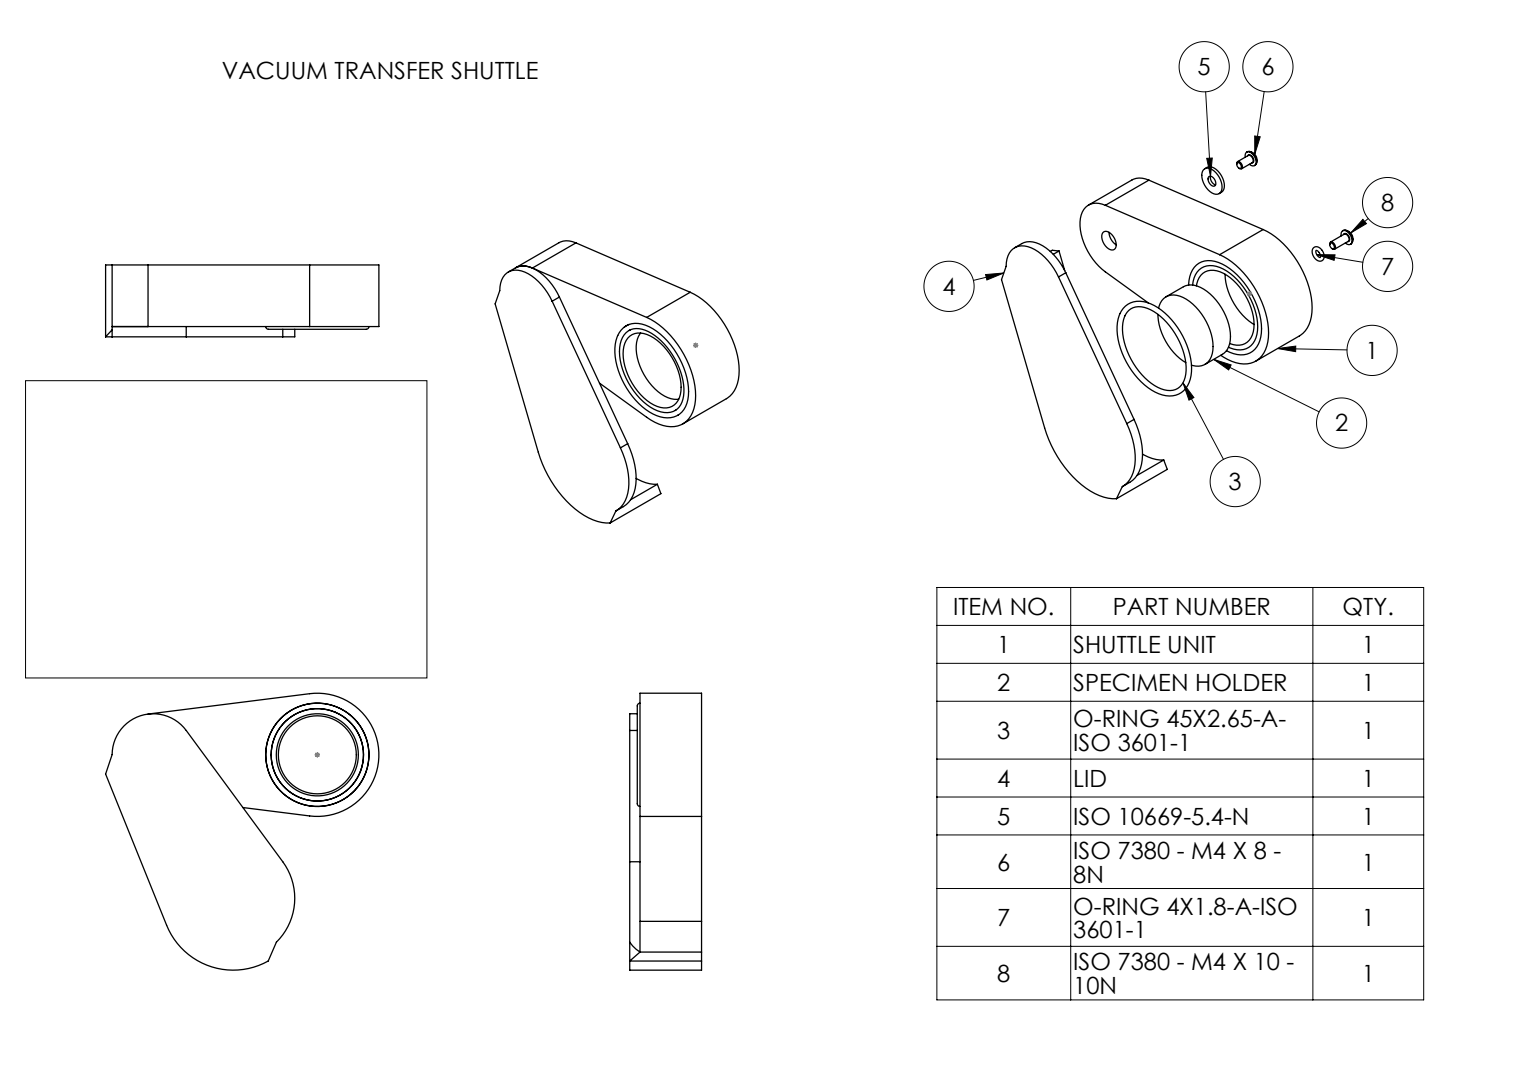
ISO-10303-21;
HEADER;
FILE_DESCRIPTION (('STEP AP214'),
    '1' );
FILE_NAME ('MAS-190',
    '2026-10-24T08:20:21',
    ( '' ),
    ( '' ),
    'SwSTEP 2.0',
    'SolidWorks 2026',
    '' );
FILE_SCHEMA (( 'AUTOMOTIVE_DESIGN' ));
ENDSEC;

DATA;
#1 = VERTEX_POINT ( 'NONE', #624 ) ;
#2 = DIRECTION ( 'NONE',  ( -1.000000000000000000, 0.000000000000000000, 0.000000000000000000 ) ) ;
#3 = CARTESIAN_POINT ( 'NONE',  ( 1.300000000000000044, 1.443375672974065216, 7.222237291452134449E-31 ) ) ;
#4 = DIRECTION ( 'NONE',  ( -0.000000000000000000, -0.000000000000000000, -1.000000000000000000 ) ) ;
#5 = ORIENTED_EDGE ( 'NONE', *, *, #1076, .T. ) ;
#6 = CARTESIAN_POINT ( 'NONE',  ( 0.000000000000000000, 0.000000000000000000, -15.70000000000000284 ) ) ;
#7 = PLANE ( 'NONE',  #3620 ) ;
#8 = DIRECTION ( 'NONE',  ( 1.000000000000000000, 0.000000000000000000, 0.000000000000000000 ) ) ;
#9 = DIRECTION ( 'NONE',  ( 0.000000000000000000, 0.000000000000000000, 1.000000000000000000 ) ) ;
#10 = ORIENTED_EDGE ( 'NONE', *, *, #2629, .T. ) ;
#11 = ORIENTED_EDGE ( 'NONE', *, *, #3486, .F. ) ;
#12 = LINE ( 'NONE', #3823, #2390 ) ;
#13 = ORIENTED_EDGE ( 'NONE', *, *, #231, .T. ) ;
#14 = CARTESIAN_POINT ( 'NONE',  ( 1.820000000000000062, 0.000000000000000000, 0.000000000000000000 ) ) ;
#15 = VERTEX_POINT ( 'NONE', #148 ) ;
#16 = CARTESIAN_POINT ( 'NONE',  ( 0.000000000000000000, 8.572527594031473190E-16, -7.000000000000000000 ) ) ;
#17 = DIRECTION ( 'NONE',  ( -1.000000000000000000, -1.224646799147353454E-16, 0.000000000000000000 ) ) ;
#18 = VECTOR ( 'NONE', #3561, 1000.000000000000114 ) ;
#19 = DIRECTION ( 'NONE',  ( -0.7071067811865492381, 8.659560562354911904E-17, -0.7071067811865457964 ) ) ;
#20 = AXIS2_PLACEMENT_3D ( 'NONE', #499, #4, #521 ) ;
#21 = EDGE_LOOP ( 'NONE', ( #2313, #294, #1297, #1026, #1998 ) ) ;
#22 = CARTESIAN_POINT ( 'NONE',  ( 0.000000000000000000, 0.000000000000000000, -30.00000000000000000 ) ) ;
#23 = LINE ( 'NONE', #2105, #2068 ) ;
#24 = VECTOR ( 'NONE', #1964, 1000.000000000000000 ) ;
#25 = VECTOR ( 'NONE', #749, 1000.000000000000114 ) ;
#26 = EDGE_CURVE ( 'NONE', #192, #3050, #3399, .T. ) ;
#27 = CARTESIAN_POINT ( 'NONE',  ( -85.00000000000000000, 6.123233995736770227E-16, 0.000000000000000000 ) ) ;
#28 = EDGE_LOOP ( 'NONE', ( #1681, #1312, #3374, #1579 ) ) ;
#29 = VECTOR ( 'NONE', #2095, 1000.000000000000000 ) ;
#30 = ORIENTED_EDGE ( 'NONE', *, *, #1022, .T. ) ;
#31 = EDGE_LOOP ( 'NONE', ( #3797, #723, #569, #2340, #3263 ) ) ;
#32 = LINE ( 'NONE', #599, #2631 ) ;
#33 = CIRCLE ( 'NONE', #906, 20.00000000000000355 ) ;
#34 = EDGE_CURVE ( 'NONE', #3645, #1107, #2841, .T. ) ;
#35 = CIRCLE ( 'NONE', #2208, 22.50000000000000355 ) ;
#36 = ORIENTED_EDGE ( 'NONE', *, *, #1121, .F. ) ;
#37 = FACE_OUTER_BOUND ( 'NONE', #2030, .T. ) ;
#38 = CARTESIAN_POINT ( 'NONE',  ( 0.000000000000000000, -0.7216878364870318308, -1.250000000000000000 ) ) ;
#39 = CARTESIAN_POINT ( 'NONE',  ( 0.000000000000000000, 0.000000000000000000, -24.90000000000000568 ) ) ;
#40 = COLOUR_RGB ( '',0.8941176470588234615, 0.8941176470588234615, 0.8941176470588234615 ) ;
#41 = PRODUCT_DEFINITION_SHAPE ( 'NONE', 'NONE',  #583 ) ;
#42 = DIRECTION ( 'NONE',  ( 0.000000000000000000, 0.000000000000000000, 1.000000000000000000 ) ) ;
#43 = PLANE ( 'NONE',  #1656 ) ;
#44 = DIRECTION ( 'NONE',  ( -0.000000000000000000, 0.5000000000000002220, -0.8660254037844384856 ) ) ;
#45 =( LENGTH_UNIT ( ) NAMED_UNIT ( * ) SI_UNIT ( .MILLI., .METRE. ) );
#46 = EDGE_CURVE ( 'NONE', #2758, #1577, #1662, .T. ) ;
#47 = PLANE ( 'NONE',  #2813 ) ;
#48 = CARTESIAN_POINT ( 'NONE',  ( 1.300000000000000044, 0.000000000000000000, 0.000000000000000000 ) ) ;
#49 = EDGE_CURVE ( 'NONE', #3210, #3147, #1369, .T. ) ;
#50 = ORIENTED_EDGE ( 'NONE', *, *, #3736, .T. ) ;
#51 = FACE_OUTER_BOUND ( 'NONE', #2108, .T. ) ;
#52 = VERTEX_POINT ( 'NONE', #3188 ) ;
#53 = CARTESIAN_POINT ( 'NONE',  ( 2.021687836487040535, 0.000000000000000000, 2.168404344971008868E-16 ) ) ;
#54 = ORIENTED_EDGE ( 'NONE', *, *, #3614, .T. ) ;
#55 = DIRECTION ( 'NONE',  ( 1.000000000000000000, 0.000000000000000000, 0.000000000000000000 ) ) ;
#56 = DIRECTION ( 'NONE',  ( -1.000000000000000000, 0.000000000000000000, -0.000000000000000000 ) ) ;
#57 = CARTESIAN_POINT ( 'NONE',  ( 2.200000000000000178, 0.000000000000000000, 3.799999999999999378 ) ) ;
#58 = DIRECTION ( 'NONE',  ( 0.1250000000000000833, 0.9921567416492215186, -0.000000000000000000 ) ) ;
#59 = DIRECTION ( 'NONE',  ( 1.000000000000000000, 0.000000000000000000, 0.000000000000000000 ) ) ;
#60 = DIRECTION ( 'NONE',  ( 1.000000000000000000, 0.000000000000000000, -0.000000000000000000 ) ) ;
#61 = DIRECTION ( 'NONE',  ( -1.000000000000000000, -1.224646799147352961E-16, 0.000000000000000000 ) ) ;
#62 = AXIS2_PLACEMENT_3D ( 'NONE', #1095, #2604, #3467 ) ;
#63 = ORIENTED_EDGE ( 'NONE', *, *, #1690, .T. ) ;
#64 = DIRECTION ( 'NONE',  ( -1.000000000000000000, 0.000000000000000000, 0.000000000000000000 ) ) ;
#65 = EDGE_LOOP ( 'NONE', ( #2892, #2887, #2094, #2492 ) ) ;
#66 = CARTESIAN_POINT ( 'NONE',  ( -80.00000000000000000, 0.000000000000000000, -5.000000000000000000 ) ) ;
#67 = ORIENTED_EDGE ( 'NONE', *, *, #1212, .F. ) ;
#68 = CARTESIAN_POINT ( 'NONE',  ( -80.00000000000000000, 0.000000000000000000, 0.000000000000000000 ) ) ;
#69 = FACE_OUTER_BOUND ( 'NONE', #2614, .T. ) ;
#70 = DIRECTION ( 'NONE',  ( -1.000000000000000000, 0.000000000000000000, 0.000000000000000000 ) ) ;
#71 = AXIS2_PLACEMENT_3D ( 'NONE', #2197, #416, #1075 ) ;
#72 = CARTESIAN_POINT ( 'NONE',  ( 1.300000000000000044, -0.7216878364870317197, -1.250000000000000000 ) ) ;
#73 = CARTESIAN_POINT ( 'NONE',  ( -80.00000000000000000, 0.000000000000000000, -5.000000000000000000 ) ) ;
#74 = TOROIDAL_SURFACE ( 'NONE', #3494, 23.82500000000000284, 1.324999999999999956 ) ;
#75 = VECTOR ( 'NONE', #2409, 1000.000000000000114 ) ;
#76 = FACE_OUTER_BOUND ( 'NONE', #2053, .T. ) ;
#77 = DIRECTION ( 'NONE',  ( -1.000000000000000000, 0.000000000000000000, 0.000000000000000000 ) ) ;
#78 = EDGE_CURVE ( 'NONE', #2558, #3229, #1744, .T. ) ;
#79 = VECTOR ( 'NONE', #1201, 1000.000000000000000 ) ;
#80 = VERTEX_POINT ( 'NONE', #800 ) ;
#81 = SURFACE_STYLE_USAGE ( .BOTH. , #2750 ) ;
#82 = ORIENTED_EDGE ( 'NONE', *, *, #2472, .F. ) ;
#83 = AXIS2_PLACEMENT_3D ( 'NONE', #3751, #2911, #1411 ) ;
#84 = DIRECTION ( 'NONE',  ( -1.000000000000000000, -0.000000000000000000, -0.000000000000000000 ) ) ;
#85 = CARTESIAN_POINT ( 'NONE',  ( 0.000000000000000000, 0.000000000000000000, -30.00000000000000000 ) ) ;
#86 = ORIENTED_EDGE ( 'NONE', *, *, #1066, .F. ) ;
#87 = CARTESIAN_POINT ( 'NONE',  ( 0.000000000000000000, 0.000000000000000000, 0.000000000000000000 ) ) ;
#88 = VECTOR ( 'NONE', #755, 999.9999999999998863 ) ;
#89 = CARTESIAN_POINT ( 'NONE',  ( 0.000000000000000000, 0.000000000000000000, -15.70000000000000284 ) ) ;
#90 = AXIS2_PLACEMENT_3D ( 'NONE', #3655, #2505, #3718 ) ;
#91 = LINE ( 'NONE', #72, #1895 ) ;
#92 = CARTESIAN_POINT ( 'NONE',  ( 28.92857142857272379, 7.945926950454914817, 5.000000000000000000 ) ) ;
#93 = AXIS2_PLACEMENT_3D ( 'NONE', #3300, #56, #338 ) ;
#94 = CARTESIAN_POINT ( 'NONE',  ( 0.000000000000000000, 0.000000000000000000, 1.999999999999999112 ) ) ;
#95 = CARTESIAN_POINT ( 'NONE',  ( 1.600000000000000089, 0.000000000000000000, 0.000000000000000000 ) ) ;
#96 = ORIENTED_EDGE ( 'NONE', *, *, #3202, .F. ) ;
#97 = ORIENTED_EDGE ( 'NONE', *, *, #3095, .F. ) ;
#98 = CARTESIAN_POINT ( 'NONE',  ( 1.300000000000000044, -0.7216878364870317197, -1.250000000000000000 ) ) ;
#99 = ADVANCED_FACE ( 'NONE', ( #3496 ), #810, .T. ) ;
#100 = EDGE_CURVE ( 'NONE', #2912, #2597, #2303, .T. ) ;
#101 = CARTESIAN_POINT ( 'NONE',  ( -85.00000000000000000, 0.000000000000000000, 0.001000000000000132727 ) ) ;
#102 = VERTEX_POINT ( 'NONE', #209 ) ;
#103 = CARTESIAN_POINT ( 'NONE',  ( -90.00000000000000000, 0.000000000000000000, -4.999999999999997335 ) ) ;
#104 = FACE_OUTER_BOUND ( 'NONE', #1200, .T. ) ;
#105 = DIRECTION ( 'NONE',  ( -1.000000000000000000, 0.000000000000000000, 0.000000000000000000 ) ) ;
#106 = EDGE_CURVE ( 'NONE', #1824, #3785, #3518, .T. ) ;
#107 = CARTESIAN_POINT ( 'NONE',  ( -82.50000000000000000, -19.84313483298442904, 0.000000000000000000 ) ) ;
#108 = ORIENTED_EDGE ( 'NONE', *, *, #561, .F. ) ;
#109 = DIRECTION ( 'NONE',  ( -1.000000000000000000, -0.000000000000000000, -0.000000000000000000 ) ) ;
#110 = ADVANCED_FACE ( 'NONE', ( #3446, #2287 ), #2899, .F. ) ;
#111 = DIRECTION ( 'NONE',  ( -0.000000000000000000, -0.000000000000000000, -1.000000000000000000 ) ) ;
#112 = PLANE ( 'NONE',  #3812 ) ;
#113 = ORIENTED_EDGE ( 'NONE', *, *, #1158, .T. ) ;
#114 =( NAMED_UNIT ( * ) SI_UNIT ( $, .STERADIAN. ) SOLID_ANGLE_UNIT ( ) );
#115 = ORIENTED_EDGE ( 'NONE', *, *, #3737, .T. ) ;
#116 = PLANE ( 'NONE',  #1634 ) ;
#117 = CARTESIAN_POINT ( 'NONE',  ( 1.820000000000000062, 3.799999999999999378, 0.000000000000000000 ) ) ;
#118 = ORIENTED_EDGE ( 'NONE', *, *, #270, .T. ) ;
#119 = DIRECTION ( 'NONE',  ( -0.000000000000000000, 0.000000000000000000, 1.000000000000000000 ) ) ;
#120 = CARTESIAN_POINT ( 'NONE',  ( 12.20000000000000107, 0.000000000000000000, 0.000000000000000000 ) ) ;
#121 = PLANE ( 'NONE',  #644 ) ;
#122 = CARTESIAN_POINT ( 'NONE',  ( 9.809999999999998721, 0.000000000000000000, 0.000000000000000000 ) ) ;
#123 = EDGE_LOOP ( 'NONE', ( #2898, #2234 ) ) ;
#124 = LINE ( 'NONE', #2843, #702 ) ;
#125 = SURFACE_STYLE_USAGE ( .BOTH. , #2878 ) ;
#126 = CIRCLE ( 'NONE', #71, 1.999999999999999556 ) ;
#127 = APPLICATION_PROTOCOL_DEFINITION ( 'draft international standard', 'automotive_design', 1998, #1375 ) ;
#128 = CARTESIAN_POINT ( 'NONE',  ( -80.00000000000000000, 0.000000000000000000, -30.00000000000000000 ) ) ;
#129 = CARTESIAN_POINT ( 'NONE',  ( 1.300000000000000044, 0.7216878364870328300, -1.250000000000000000 ) ) ;
#130 = COLOUR_RGB ( '',0.8941176470588234615, 0.8941176470588234615, 0.8941176470588234615 ) ;
#131 = VECTOR ( 'NONE', #1399, 1000.000000000000000 ) ;
#132 = AXIS2_PLACEMENT_3D ( 'NONE', #1292, #3708, #687 ) ;
#133 =( GEOMETRIC_REPRESENTATION_CONTEXT ( 3 ) GLOBAL_UNCERTAINTY_ASSIGNED_CONTEXT ( ( #1987 ) ) GLOBAL_UNIT_ASSIGNED_CONTEXT ( ( #3301, #2413, #2158 ) ) REPRESENTATION_CONTEXT ( 'NONE', 'WORKASPACE' ) );
#134 = EDGE_CURVE ( 'NONE', #1873, #2443, #3640, .T. ) ;
#135 = EDGE_LOOP ( 'NONE', ( #399, #815 ) ) ;
#136 = CARTESIAN_POINT ( 'NONE',  ( 1.300000000000000044, -1.082531754730548412, -0.6249999999999997780 ) ) ;
#137 = VERTEX_POINT ( 'NONE', #2620 ) ;
#138 = CARTESIAN_POINT ( 'NONE',  ( -83.12500000000000000, -24.80391854123052653, 5.000000000000000000 ) ) ;
#139 = CIRCLE ( 'NONE', #3685, 1.250000000000000222 ) ;
#140 = VECTOR ( 'NONE', #2256, 1000.000000000000000 ) ;
#141 = VECTOR ( 'NONE', #617, 1000.000000000000000 ) ;
#142 = FACE_OUTER_BOUND ( 'NONE', #2988, .T. ) ;
#143 = VERTEX_POINT ( 'NONE', #2588 ) ;
#144 = DIRECTION ( 'NONE',  ( 1.000000000000000000, 0.000000000000000000, 0.000000000000000000 ) ) ;
#145 = EDGE_CURVE ( 'NONE', #3052, #3455, #33, .T. ) ;
#146 = DIRECTION ( 'NONE',  ( 0.000000000000000000, 0.8660254037844385966, -0.5000000000000003331 ) ) ;
#147 = DIRECTION ( 'NONE',  ( -1.000000000000000000, -0.000000000000000000, -0.000000000000000000 ) ) ;
#148 = CARTESIAN_POINT ( 'NONE',  ( -1.649999999999999911, 0.000000000000000000, -15.70000000000000284 ) ) ;
#149 = FACE_OUTER_BOUND ( 'NONE', #2973, .T. ) ;
#150 = AXIS2_PLACEMENT_3D ( 'NONE', #3676, #1911, #3108 ) ;
#151 = EDGE_CURVE ( 'NONE', #2912, #447, #915, .T. ) ;
#152 =( REPRESENTATION_RELATIONSHIP ('NONE','NONE', #681, #556 ) REPRESENTATION_RELATIONSHIP_WITH_TRANSFORMATION ( #1484 )SHAPE_REPRESENTATION_RELATIONSHIP( ) );
#153 = COLOUR_RGB ( '',1.000000000000000000, 0.9490196078431372140, 0.9098039215686274384 ) ;
#154 = CIRCLE ( 'NONE', #90, 3.799999999999999378 ) ;
#155 = FACE_OUTER_BOUND ( 'NONE', #841, .T. ) ;
#156 = CARTESIAN_POINT ( 'NONE',  ( 9.809999999999998721, 2.449293598294705921E-16, -1.999999999999999556 ) ) ;
#157 = EDGE_CURVE ( 'NONE', #2149, #2587, #627, .T. ) ;
#158 = VECTOR ( 'NONE', #3390, 1000.000000000000000 ) ;
#159 = SHAPE_REPRESENTATION ( 'shuttle unit', ( #2207 ), #968 ) ;
#160 = ORIENTED_EDGE ( 'NONE', *, *, #2560, .F. ) ;
#161 = EDGE_LOOP ( 'NONE', ( #2165, #1220, #1169, #2717, #1654 ) ) ;
#162 = EDGE_CURVE ( 'NONE', #3091, #1782, #1381, .T. ) ;
#163 = DIRECTION ( 'NONE',  ( 0.000000000000000000, 0.000000000000000000, -1.000000000000000000 ) ) ;
#164 = EDGE_CURVE ( 'NONE', #494, #1780, #3780, .T. ) ;
#165 = PRODUCT_DEFINITION_CONTEXT ( 'detailed design', #1421, 'design' ) ;
#166 = CARTESIAN_POINT ( 'NONE',  ( 20.00000000000000000, 0.000000000000000000, 0.000000000000000000 ) ) ;
#167 = ORIENTED_EDGE ( 'NONE', *, *, #1783, .T. ) ;
#168 = DIRECTION ( 'NONE',  ( 0.000000000000000000, 0.000000000000000000, -1.000000000000000000 ) ) ;
#169 = CARTESIAN_POINT ( 'NONE',  ( 11.80999999999999872, 0.000000000000000000, 0.000000000000000000 ) ) ;
#170 = CARTESIAN_POINT ( 'NONE',  ( 10.20000000000000107, 0.000000000000000000, 1.610000000000000098 ) ) ;
#171 = ORIENTED_EDGE ( 'NONE', *, *, #2472, .T. ) ;
#172 = ORIENTED_EDGE ( 'NONE', *, *, #567, .F. ) ;
#173 = DIRECTION ( 'NONE',  ( 0.000000000000000000, 0.000000000000000000, 1.000000000000000000 ) ) ;
#174 =( NAMED_UNIT ( * ) PLANE_ANGLE_UNIT ( ) SI_UNIT ( $, .RADIAN. ) );
#175 = DIRECTION ( 'NONE',  ( -0.000000000000000000, -0.4999999999999999445, -0.8660254037844387076 ) ) ;
#176 = CARTESIAN_POINT ( 'NONE',  ( 0.000000000000000000, 0.000000000000000000, -30.00000000000000000 ) ) ;
#177 = ADVANCED_FACE ( 'NONE', ( #484 ), #3479, .T. ) ;
#178 = ORIENTED_EDGE ( 'NONE', *, *, #1295, .F. ) ;
#179 = CARTESIAN_POINT ( 'NONE',  ( -80.00000000000000000, 0.000000000000000000, 0.001000000000000132727 ) ) ;
#180 = ORIENTED_EDGE ( 'NONE', *, *, #2925, .T. ) ;
#181 = FACE_OUTER_BOUND ( 'NONE', #2792, .T. ) ;
#182 = DIRECTION ( 'NONE',  ( -0.000000000000000000, 0.000000000000000000, 1.000000000000000000 ) ) ;
#183 = ORIENTED_EDGE ( 'NONE', *, *, #151, .F. ) ;
#184 = LINE ( 'NONE', #240, #851 ) ;
#185 = CARTESIAN_POINT ( 'NONE',  ( 0.000000000000000000, 0.000000000000000000, 0.000000000000000000 ) ) ;
#186 = ORIENTED_EDGE ( 'NONE', *, *, #1295, .T. ) ;
#187 = CARTESIAN_POINT ( 'NONE',  ( -82.50000000000000000, -19.84313483298442904, 0.000000000000000000 ) ) ;
#188 = PLANE ( 'NONE',  #436 ) ;
#189 = PRODUCT_CONTEXT ( 'NONE', #958, 'mechanical' ) ;
#190 = DIRECTION ( 'NONE',  ( -0.000000000000000000, 0.000000000000000000, 1.000000000000000000 ) ) ;
#191 = EDGE_CURVE ( 'NONE', #3559, #2247, #1971, .T. ) ;
#192 = VERTEX_POINT ( 'NONE', #3809 ) ;
#193 = CONICAL_SURFACE ( 'NONE', #3677, 1732.050807568856271, 1.047197551196592524 ) ;
#194 = FACE_OUTER_BOUND ( 'NONE', #457, .T. ) ;
#195 = ORIENTED_EDGE ( 'NONE', *, *, #970, .T. ) ;
#196 = EDGE_CURVE ( 'NONE', #673, #620, #3793, .T. ) ;
#197 = CIRCLE ( 'NONE', #701, 0.2000000000000000944 ) ;
#198 =( GEOMETRIC_REPRESENTATION_CONTEXT ( 3 ) GLOBAL_UNCERTAINTY_ASSIGNED_CONTEXT ( ( #1403 ) ) GLOBAL_UNIT_ASSIGNED_CONTEXT ( ( #953, #339, #637 ) ) REPRESENTATION_CONTEXT ( 'NONE', 'WORKASPACE' ) );
#199 = PRODUCT_DEFINITION_CONTEXT ( 'detailed design', #1821, 'design' ) ;
#200 = DIRECTION ( 'NONE',  ( 0.000000000000000000, 0.000000000000000000, 1.000000000000000000 ) ) ;
#201 = VERTEX_POINT ( 'NONE', #243 ) ;
#202 = CARTESIAN_POINT ( 'NONE',  ( 28.92857142857272379, 7.945926950454914817, 5.000000000000000000 ) ) ;
#203 = MECHANICAL_DESIGN_GEOMETRIC_PRESENTATION_REPRESENTATION (  '', ( #1878 ), #378 ) ;
#204 = AXIS2_PLACEMENT_3D ( 'NONE', #554, #3183, #2954 ) ;
#205 = CYLINDRICAL_SURFACE ( 'NONE', #444, 2.700000000000000178 ) ;
#206 = EDGE_CURVE ( 'NONE', #535, #3277, #1093, .T. ) ;
#207 = AXIS2_PLACEMENT_3D ( 'NONE', #2463, #2835, #972 ) ;
#208 = VERTEX_POINT ( 'NONE', #3226 ) ;
#209 = CARTESIAN_POINT ( 'NONE',  ( 10.20000000000000107, 2.210487472460972205E-16, -1.610000000000000098 ) ) ;
#210 = DIRECTION ( 'NONE',  ( 1.000000000000000000, 0.000000000000000000, 0.000000000000000000 ) ) ;
#211 = TOROIDAL_SURFACE ( 'NONE', #83, 23.82500000000000284, 1.324999999999999956 ) ;
#212 = PLANE ( 'NONE',  #3487 ) ;
#213 = AXIS2_PLACEMENT_3D ( 'NONE', #1985, #1430, #779 ) ;
#214 = PRESENTATION_LAYER_ASSIGNMENT (  '', '', ( #2141 ) ) ;
#215 = CIRCLE ( 'NONE', #1581, 4.500000000000000888 ) ;
#216 = ORIENTED_EDGE ( 'NONE', *, *, #1379, .F. ) ;
#217 = CARTESIAN_POINT ( 'NONE',  ( -85.13135963406439544, -19.37413418176162594, 2.144658748104447454 ) ) ;
#218 = ORIENTED_EDGE ( 'NONE', *, *, #3772, .F. ) ;
#219 = VECTOR ( 'NONE', #404, 1000.000000000000000 ) ;
#220 = PRODUCT_DEFINITION_FORMATION_WITH_SPECIFIED_SOURCE ( 'ANY', '', #2168, .NOT_KNOWN. ) ;
#221 = AXIS2_PLACEMENT_3D ( 'NONE', #1149, #559, #3521 ) ;
#222 = FACE_OUTER_BOUND ( 'NONE', #2249, .T. ) ;
#223 = ORIENTED_EDGE ( 'NONE', *, *, #2872, .T. ) ;
#224 = DIRECTION ( 'NONE',  ( 0.000000000000000000, -1.000000000000000000, 0.000000000000000000 ) ) ;
#225 = DIRECTION ( 'NONE',  ( -1.000000000000000000, -0.000000000000000000, -0.000000000000000000 ) ) ;
#226 = ORIENTED_EDGE ( 'NONE', *, *, #2070, .F. ) ;
#227 = DIRECTION ( 'NONE',  ( -0.000000000000000000, -0.000000000000000000, -1.000000000000000000 ) ) ;
#228 = CARTESIAN_POINT ( 'NONE',  ( -80.00000000000000000, 0.000000000000000000, -5.000000000000000000 ) ) ;
#229 = SURFACE_STYLE_USAGE ( .BOTH. , #3555 ) ;
#230 = EDGE_LOOP ( 'NONE', ( #423, #458, #2940, #857 ) ) ;
#231 = EDGE_CURVE ( 'NONE', #2038, #698, #2551, .T. ) ;
#232 = LINE ( 'NONE', #2626, #1435 ) ;
#233 = SURFACE_SIDE_STYLE ('',( #1990 ) ) ;
#234 = DIRECTION ( 'NONE',  ( -0.000000000000000000, -0.5000000000000002220, -0.8660254037844384856 ) ) ;
#235 = ORIENTED_EDGE ( 'NONE', *, *, #2182, .F. ) ;
#236 = B_SPLINE_CURVE_WITH_KNOTS ( 'NONE', 3,
 ( #2282, #3465, #1982, #3172 ),
 .UNSPECIFIED., .F., .F.,
 ( 4, 4 ),
 ( 0.000000000000000000, 1.000000000000000000 ),
 .UNSPECIFIED. ) ;
#237 = ADVANCED_FACE ( 'NONE', ( #1844, #3552 ), #2668, .F. ) ;
#238 = PLANE ( 'NONE',  #1875 ) ;
#239 = ORIENTED_EDGE ( 'NONE', *, *, #1254, .T. ) ;
#240 = CARTESIAN_POINT ( 'NONE',  ( -4.374999999999999112, -34.72548595772274638, -30.00000000000000000 ) ) ;
#241 = CARTESIAN_POINT ( 'NONE',  ( 4.336808689942017736E-16, -0.7216878364870318308, 1.249999999999999778 ) ) ;
#242 = EDGE_LOOP ( 'NONE', ( #1908, #2671, #1653, #2183 ) ) ;
#243 = CARTESIAN_POINT ( 'NONE',  ( 0.000000000000000000, 0.000000000000000000, 7.000000000000000000 ) ) ;
#244 =( NAMED_UNIT ( * ) PLANE_ANGLE_UNIT ( ) SI_UNIT ( $, .RADIAN. ) );
#245 = PRODUCT_RELATED_PRODUCT_CATEGORY ( 'part', '', ( #2168 ) ) ;
#246 = EDGE_LOOP ( 'NONE', ( #195, #3218 ) ) ;
#247 = FACE_BOUND ( 'NONE', #351, .T. ) ;
#248 = CARTESIAN_POINT ( 'NONE',  ( -4.375000000000000888, -34.72548595772274638, 5.000000000000000000 ) ) ;
#249 = ORIENTED_EDGE ( 'NONE', *, *, #1970, .F. ) ;
#250 = ADVANCED_FACE ( 'NONE', ( #2060 ), #299, .T. ) ;
#251 = CIRCLE ( 'NONE', #760, 18.99999999999999645 ) ;
#252 = EDGE_LOOP ( 'NONE', ( #3787, #1790, #3683, #1738 ) ) ;
#253 = DIRECTION ( 'NONE',  ( -1.000000000000000000, -0.000000000000000000, -0.000000000000000000 ) ) ;
#254 = ORIENTED_EDGE ( 'NONE', *, *, #3594, .F. ) ;
#255 = DIRECTION ( 'NONE',  ( 0.000000000000000000, 0.000000000000000000, 1.000000000000000000 ) ) ;
#256 = CYLINDRICAL_SURFACE ( 'NONE', #2880, 20.00000000000000000 ) ;
#257=STYLED_ITEM('',(#3881),#1995);
#258 = AXIS2_PLACEMENT_3D ( 'NONE', #2656, #623, #2632 ) ;
#259 = CIRCLE ( 'NONE', #954, 3.799999999999999378 ) ;
#260 = SHAPE_DEFINITION_REPRESENTATION ( #1206, #556 ) ;
#261 = VERTEX_POINT ( 'NONE', #657 ) ;
#262 = DIRECTION ( 'NONE',  ( 0.000000000000000000, 0.000000000000000000, 1.000000000000000000 ) ) ;
#263 = AXIS2_PLACEMENT_3D ( 'NONE', #1547, #656, #1261 ) ;
#264 = ORIENTED_EDGE ( 'NONE', *, *, #1371, .T. ) ;
#265 = CARTESIAN_POINT ( 'NONE',  ( 1.300000000000000044, -1.082531754730548412, 0.6249999999999998890 ) ) ;
#266 = TOROIDAL_SURFACE ( 'NONE', #3014, 2.199999999999999289, 0.2000000000000000111 ) ;
#267 = FACE_OUTER_BOUND ( 'NONE', #1466, .T. ) ;
#268 =( LENGTH_UNIT ( ) NAMED_UNIT ( * ) SI_UNIT ( .MILLI., .METRE. ) );
#269 = B_SPLINE_CURVE_WITH_KNOTS ( 'NONE', 3,
 ( #2225, #1680, #3784, #502 ),
 .UNSPECIFIED., .F., .F.,
 ( 4, 4 ),
 ( 0.000000000000000000, 1.000000000000000000 ),
 .UNSPECIFIED. ) ;
#270 = EDGE_CURVE ( 'NONE', #1478, #2858, #2967, .T. ) ;
#271 = LINE ( 'NONE', #3543, #2440 ) ;
#272 = VERTEX_POINT ( 'NONE', #897 ) ;
#273 = AXIS2_PLACEMENT_3D ( 'NONE', #2448, #3041, #3118 ) ;
#274 = ORIENTED_EDGE ( 'NONE', *, *, #2686, .T. ) ;
#275 = EDGE_CURVE ( 'NONE', #1577, #1374, #3092, .T. ) ;
#276 = VERTEX_POINT ( 'NONE', #1202 ) ;
#277 = CARTESIAN_POINT ( 'NONE',  ( 1.600000000000000089, 0.000000000000000000, 2.700000000000000178 ) ) ;
#278 = ADVANCED_FACE ( 'NONE', ( #3617 ), #2093, .F. ) ;
#279 = VECTOR ( 'NONE', #1163, 1000.000000000000000 ) ;
#280 = DIRECTION ( 'NONE',  ( -0.000000000000000000, -0.000000000000000000, -1.000000000000000000 ) ) ;
#281 = ORIENTED_EDGE ( 'NONE', *, *, #3302, .F. ) ;
#282 = SHAPE_REPRESENTATION ( 'o-rings series a_iso_O-ring 4x1.8-A-ISO 3601-1', ( #2207 ), #2896 ) ;
#283 = VERTEX_POINT ( 'NONE', #3 ) ;
#284 = DIRECTION ( 'NONE',  ( 1.000000000000000000, 0.000000000000000000, -0.000000000000000000 ) ) ;
#285 = DIRECTION ( 'NONE',  ( -1.000000000000000000, 0.000000000000000000, 0.000000000000000000 ) ) ;
#286 = FACE_OUTER_BOUND ( 'NONE', #2486, .T. ) ;
#287 = PRESENTATION_STYLE_ASSIGNMENT (( #2918 ) ) ;
#288 = B_SPLINE_CURVE_WITH_KNOTS ( 'NONE', 3,
 ( #1129, #864, #2961, #3833 ),
 .UNSPECIFIED., .F., .F.,
 ( 4, 4 ),
 ( 0.000000000000000000, 1.000000000000000000 ),
 .UNSPECIFIED. ) ;
#289 = ORIENTED_EDGE ( 'NONE', *, *, #46, .F. ) ;
#290 = DIRECTION ( 'NONE',  ( 0.000000000000000000, 0.000000000000000000, 1.000000000000000000 ) ) ;
#291 = DIRECTION ( 'NONE',  ( 1.000000000000000000, 0.000000000000000000, 0.000000000000000000 ) ) ;
#292 = DIRECTION ( 'NONE',  ( 0.000000000000000000, 0.000000000000000000, 1.000000000000000000 ) ) ;
#293 = EDGE_LOOP ( 'NONE', ( #2519, #1807, #3422, #686 ) ) ;
#294 = ORIENTED_EDGE ( 'NONE', *, *, #561, .T. ) ;
#295 = ORIENTED_EDGE ( 'NONE', *, *, #2901, .F. ) ;
#296 = CARTESIAN_POINT ( 'NONE',  ( 23.18826319173439288, -9.737913028511604452, 0.000000000000000000 ) ) ;
#297 = ORIENTED_EDGE ( 'NONE', *, *, #1259, .F. ) ;
#298 = CARTESIAN_POINT ( 'NONE',  ( 1.300000000000000044, 0.7216878364870328300, -1.250000000000000000 ) ) ;
#299 = CYLINDRICAL_SURFACE ( 'NONE', #1463, 20.00000000000000355 ) ;
#300 = EDGE_CURVE ( 'NONE', #3067, #2698, #472, .T. ) ;
#301 = ORIENTED_EDGE ( 'NONE', *, *, #2925, .F. ) ;
#302 = FACE_OUTER_BOUND ( 'NONE', #2329, .T. ) ;
#303 = FACE_OUTER_BOUND ( 'NONE', #3792, .T. ) ;
#304 = EDGE_CURVE ( 'NONE', #2072, #2934, #2995, .T. ) ;
#305 = DIRECTION ( 'NONE',  ( -0.9921567416492215186, 0.1250000000000000833, 0.000000000000000000 ) ) ;
#306 = EDGE_LOOP ( 'NONE', ( #2682, #2580, #1353, #1330 ) ) ;
#307 = ORIENTED_EDGE ( 'NONE', *, *, #1137, .F. ) ;
#308 = PLANE ( 'NONE',  #2884 ) ;
#309 = EDGE_LOOP ( 'NONE', ( #3770, #1309, #1724, #1607, #1596 ) ) ;
#310 = CARTESIAN_POINT ( 'NONE',  ( 1.300000000000000044, -1.443375672974064328, 2.168404344971008868E-16 ) ) ;
#311 = ITEM_DEFINED_TRANSFORMATION ( 'NONE', 'NONE', #912,  #2207 ) ;
#312 = ORIENTED_EDGE ( 'NONE', *, *, #486, .T. ) ;
#313 = CARTESIAN_POINT ( 'NONE',  ( 0.000000000000000000, 0.000000000000000000, 0.000000000000000000 ) ) ;
#314 = CARTESIAN_POINT ( 'NONE',  ( 10.20000000000000107, 0.000000000000000000, 0.000000000000000000 ) ) ;
#315 = SURFACE_STYLE_FILL_AREA ( #919 ) ;
#316 = CARTESIAN_POINT ( 'NONE',  ( 0.000000000000000000, 0.000000000000000000, -28.00000000000000711 ) ) ;
#317 = EDGE_CURVE ( 'NONE', #742, #102, #1576, .T. ) ;
#318 = VECTOR ( 'NONE', #1119, 999.9999999999998863 ) ;
#319 = MECHANICAL_DESIGN_GEOMETRIC_PRESENTATION_REPRESENTATION (  '', ( #257 ), #133 ) ;
#320 = CARTESIAN_POINT ( 'NONE',  ( 0.000000000000000000, 0.000000000000000000, 1.622657008870242981E-16 ) ) ;
#321 = CARTESIAN_POINT ( 'NONE',  ( 0.000000000000000000, 0.000000000000000000, -30.00000000000000000 ) ) ;
#322 = SURFACE_SIDE_STYLE ('',( #3002 ) ) ;
#323 = VECTOR ( 'NONE', #1438, 1000.000000000000114 ) ;
#324 = TOROIDAL_SURFACE ( 'NONE', #959, 2.199999999999999289, 0.2000000000000000111 ) ;
#325 = LINE ( 'NONE', #2051, #1264 ) ;
#326 = ORIENTED_EDGE ( 'NONE', *, *, #2063, .T. ) ;
#327 = AXIS2_PLACEMENT_3D ( 'NONE', #856, #2331, #1108 ) ;
#328 = VERTEX_POINT ( 'NONE', #1471 ) ;
#329 = PLANE ( 'NONE',  #132 ) ;
#330 = ORIENTED_EDGE ( 'NONE', *, *, #196, .T. ) ;
#331 = CIRCLE ( 'NONE', #3200, 1.999999999999999556 ) ;
#332 = AXIS2_PLACEMENT_3D ( 'NONE', #2007, #2609, #441 ) ;
#333 = CIRCLE ( 'NONE', #2451, 0.2000000000000000944 ) ;
#334 = AXIS2_PLACEMENT_3D ( 'NONE', #344, #1188, #42 ) ;
#335 = CONTEXT_DEPENDENT_SHAPE_REPRESENTATION ( #152, #2428 ) ;
#336 = ORIENTED_EDGE ( 'NONE', *, *, #3302, .T. ) ;
#337 = LINE ( 'NONE', #298, #2756 ) ;
#338 = DIRECTION ( 'NONE',  ( -0.000000000000000000, 0.000000000000000000, 1.000000000000000000 ) ) ;
#339 =( NAMED_UNIT ( * ) PLANE_ANGLE_UNIT ( ) SI_UNIT ( $, .RADIAN. ) );
#340 = MECHANICAL_DESIGN_GEOMETRIC_PRESENTATION_REPRESENTATION (  '', ( #468 ), #3515 ) ;
#341 = AXIS2_PLACEMENT_3D ( 'NONE', #470, #1696, #3451 ) ;
#342 = UNCERTAINTY_MEASURE_WITH_UNIT (LENGTH_MEASURE( 1.000000000000000082E-05 ), #3816, 'distance_accuracy_value', 'NONE');
#343 = PRODUCT ( 'lid', 'lid', '', ( #1165 ) ) ;
#344 = CARTESIAN_POINT ( 'NONE',  ( 1.820000000000000062, 0.000000000000000000, 0.000000000000000000 ) ) ;
#345 = DIRECTION ( 'NONE',  ( 0.000000000000000000, 0.000000000000000000, 1.000000000000000000 ) ) ;
#346 = PLANE ( 'NONE',  #504 ) ;
#347 = EDGE_CURVE ( 'NONE', #818, #3065, #1184, .T. ) ;
#348 = DIRECTION ( 'NONE',  ( -0.000000000000000000, -0.000000000000000000, -1.000000000000000000 ) ) ;
#349 = CARTESIAN_POINT ( 'NONE',  ( 0.000000000000000000, 0.000000000000000000, -30.00000000000000000 ) ) ;
#350 =( REPRESENTATION_RELATIONSHIP ('NONE','NONE', #681, #3744 ) REPRESENTATION_RELATIONSHIP_WITH_TRANSFORMATION ( #3239 )SHAPE_REPRESENTATION_RELATIONSHIP( ) );
#351 = EDGE_LOOP ( 'NONE', ( #1007, #874 ) ) ;
#352 = CARTESIAN_POINT ( 'NONE',  ( 2.399999999999999911, 0.000000000000000000, 0.000000000000000000 ) ) ;
#353 = ORIENTED_EDGE ( 'NONE', *, *, #1947, .T. ) ;
#354 = DIRECTION ( 'NONE',  ( -1.000000000000000000, -0.000000000000000000, -0.000000000000000000 ) ) ;
#355 = VERTEX_POINT ( 'NONE', #1451 ) ;
#356 = LINE ( 'NONE', #1470, #3071 ) ;
#357 = DIRECTION ( 'NONE',  ( -1.000000000000000000, -0.000000000000000000, -0.000000000000000000 ) ) ;
#358 = CLOSED_SHELL ( 'NONE', ( #3036, #435, #1819, #2343 ) ) ;
#359 = FILL_AREA_STYLE_COLOUR ( '', #509 ) ;
#360 = CARTESIAN_POINT ( 'NONE',  ( 1.300000000000000044, 0.7216878364870328300, -1.250000000000000000 ) ) ;
#361 = ADVANCED_FACE ( 'NONE', ( #2704, #2412, #2101 ), #1506, .T. ) ;
#362 = CYLINDRICAL_SURFACE ( 'NONE', #3771, 3.799999999999999378 ) ;
#363 = DIRECTION ( 'NONE',  ( -1.000000000000000000, 0.000000000000000000, 0.000000000000000000 ) ) ;
#364 = EDGE_LOOP ( 'NONE', ( #96, #54, #353, #289 ) ) ;
#365 = FILL_AREA_STYLE ('',( #3051 ) ) ;
#366 = ORIENTED_EDGE ( 'NONE', *, *, #3600, .F. ) ;
#367 = DIRECTION ( 'NONE',  ( 0.000000000000000000, 0.000000000000000000, 1.000000000000000000 ) ) ;
#368 = EDGE_CURVE ( 'NONE', #1824, #1740, #3586, .T. ) ;
#369 = DIRECTION ( 'NONE',  ( -1.000000000000000000, 0.000000000000000000, 0.000000000000000000 ) ) ;
#370 = EDGE_LOOP ( 'NONE', ( #10, #1130 ) ) ;
#371 = CARTESIAN_POINT ( 'NONE',  ( 34.99999999999999289, 0.000000000000000000, -30.00000000000000000 ) ) ;
#372 = DIRECTION ( 'NONE',  ( -0.9921567416492215186, 0.1250000000000000833, 0.000000000000000000 ) ) ;
#373 = SURFACE_SIDE_STYLE ('',( #3058 ) ) ;
#374 = AXIS2_PLACEMENT_3D ( 'NONE', #1676, #2860, #3740 ) ;
#375 = CARTESIAN_POINT ( 'NONE',  ( 0.000000000000000000, 0.000000000000000000, -30.00000000000000000 ) ) ;
#376 =( NAMED_UNIT ( * ) SI_UNIT ( $, .STERADIAN. ) SOLID_ANGLE_UNIT ( ) );
#377 = CIRCLE ( 'NONE', #827, 5.000000000000004441 ) ;
#378 =( GEOMETRIC_REPRESENTATION_CONTEXT ( 3 ) GLOBAL_UNCERTAINTY_ASSIGNED_CONTEXT ( ( #3167 ) ) GLOBAL_UNIT_ASSIGNED_CONTEXT ( ( #1308, #1913, #2493 ) ) REPRESENTATION_CONTEXT ( 'NONE', 'WORKASPACE' ) );
#379 = CIRCLE ( 'NONE', #1823, 9.999999999999994671 ) ;
#380 = FACE_OUTER_BOUND ( 'NONE', #736, .T. ) ;
#381 = DIRECTION ( 'NONE',  ( -0.000000000000000000, 0.000000000000000000, 1.000000000000000000 ) ) ;
#382 = EDGE_CURVE ( 'NONE', #2840, #3645, #603, .T. ) ;
#383 = VECTOR ( 'NONE', #950, 1000.000000000000114 ) ;
#384 = ORIENTED_EDGE ( 'NONE', *, *, #802, .F. ) ;
#385 = VERTEX_POINT ( 'NONE', #3241 ) ;
#386 = VECTOR ( 'NONE', #1029, 1000.000000000000000 ) ;
#387 = DIRECTION ( 'NONE',  ( -0.000000000000000000, -0.000000000000000000, -1.000000000000000000 ) ) ;
#388 = EDGE_CURVE ( 'NONE', #973, #1542, #2135, .T. ) ;
#389 = ADVANCED_FACE ( 'NONE', ( #2979, #1826 ), #580, .T. ) ;
#390 = CARTESIAN_POINT ( 'NONE',  ( 0.000000000000000000, 0.000000000000000000, -20.00000000000000000 ) ) ;
#391 = ORIENTED_EDGE ( 'NONE', *, *, #1172, .F. ) ;
#392 = CARTESIAN_POINT ( 'NONE',  ( 30.00000000000000000, 0.000000000000000000, -15.00000000000000000 ) ) ;
#393 = AXIS2_PLACEMENT_3D ( 'NONE', #1623, #717, #2482 ) ;
#394 = DIRECTION ( 'NONE',  ( -0.3871933609746165406, -0.9219985364506716463, 2.410490433790582225E-18 ) ) ;
#395 = CARTESIAN_POINT ( 'NONE',  ( 0.000000000000000000, 2.449293598294705428E-16, -1.999999999999999112 ) ) ;
#396 =( GEOMETRIC_REPRESENTATION_CONTEXT ( 3 ) GLOBAL_UNCERTAINTY_ASSIGNED_CONTEXT ( ( #342 ) ) GLOBAL_UNIT_ASSIGNED_CONTEXT ( ( #3816, #2730, #3306 ) ) REPRESENTATION_CONTEXT ( 'NONE', 'WORKASPACE' ) );
#397 = VECTOR ( 'NONE', #716, 1000.000000000000000 ) ;
#398 = CARTESIAN_POINT ( 'NONE',  ( 0.000000000000000000, -1.443375672974063884, -3.691112476943992763E-18 ) ) ;
#399 = ORIENTED_EDGE ( 'NONE', *, *, #1610, .T. ) ;
#400 = DIRECTION ( 'NONE',  ( -1.000000000000000000, -0.000000000000000000, -0.000000000000000000 ) ) ;
#401 = APPLICATION_PROTOCOL_DEFINITION ( 'draft international standard', 'automotive_design', 1998, #958 ) ;
#402 = AXIS2_PLACEMENT_3D ( 'NONE', #2062, #3244, #2606 ) ;
#403 = VECTOR ( 'NONE', #2056, 1000.000000000000000 ) ;
#404 = DIRECTION ( 'NONE',  ( -1.000000000000000000, -0.000000000000000000, -0.000000000000000000 ) ) ;
#405 = DIRECTION ( 'NONE',  ( 0.000000000000000000, 0.000000000000000000, 1.000000000000000000 ) ) ;
#406 = ORIENTED_EDGE ( 'NONE', *, *, #3273, .T. ) ;
#407 = FACE_OUTER_BOUND ( 'NONE', #796, .T. ) ;
#408 = ORIENTED_EDGE ( 'NONE', *, *, #2175, .T. ) ;
#409 = DIRECTION ( 'NONE',  ( 1.000000000000000000, 0.000000000000000000, -0.000000000000000000 ) ) ;
#410 = LINE ( 'NONE', #2154, #523 ) ;
#411 = ORIENTED_EDGE ( 'NONE', *, *, #905, .T. ) ;
#412 = LINE ( 'NONE', #3056, #2644 ) ;
#413 = LINE ( 'NONE', #3075, #777 ) ;
#414 = LINE ( 'NONE', #2795, #24 ) ;
#415 = EDGE_LOOP ( 'NONE', ( #3354, #1082 ) ) ;
#416 = DIRECTION ( 'NONE',  ( -1.000000000000000000, -0.000000000000000000, -0.000000000000000000 ) ) ;
#417 = EDGE_CURVE ( 'NONE', #3510, #535, #1487, .T. ) ;
#418 = APPLICATION_CONTEXT ( 'automotive_design' ) ;
#419 = APPLICATION_PROTOCOL_DEFINITION ( 'draft international standard', 'automotive_design', 1998, #1821 ) ;
#420 = CARTESIAN_POINT ( 'NONE',  ( 1.600000000000000089, 8.572527594031473190E-16, -7.000000000000000000 ) ) ;
#421 = LINE ( 'NONE', #1326, #1502 ) ;
#422 = EDGE_CURVE ( 'NONE', #2840, #2012, #3114, .T. ) ;
#423 = ORIENTED_EDGE ( 'NONE', *, *, #3594, .T. ) ;
#424 = ORIENTED_EDGE ( 'NONE', *, *, #368, .T. ) ;
#425 = FACE_OUTER_BOUND ( 'NONE', #911, .T. ) ;
#426 = SPHERICAL_SURFACE ( 'NONE', #1328, 4.324969328314201000 ) ;
#427 = VERTEX_POINT ( 'NONE', #2778 ) ;
#428 = LINE ( 'NONE', #2171, #969 ) ;
#429 = FACE_OUTER_BOUND ( 'NONE', #2125, .T. ) ;
#430 = CARTESIAN_POINT ( 'NONE',  ( 0.000000000000000000, 0.000000000000000000, -30.00000000000000000 ) ) ;
#431 = ADVANCED_FACE ( 'NONE', ( #104 ), #2236, .T. ) ;
#432 = DIRECTION ( 'NONE',  ( -0.000000000000000000, -0.000000000000000000, -1.000000000000000000 ) ) ;
#433 = ORIENTED_EDGE ( 'NONE', *, *, #2310, .F. ) ;
#434 = DIRECTION ( 'NONE',  ( -0.000000000000000000, -0.000000000000000000, 1.000000000000000000 ) ) ;
#435 = ADVANCED_FACE ( 'NONE', ( #429 ), #976, .T. ) ;
#436 = AXIS2_PLACEMENT_3D ( 'NONE', #459, #1382, #173 ) ;
#437 = EDGE_CURVE ( 'NONE', #427, #715, #600, .T. ) ;
#438 = APPLICATION_PROTOCOL_DEFINITION ( 'draft international standard', 'automotive_design', 1998, #418 ) ;
#439 = ADVANCED_FACE ( 'NONE', ( #3382, #69 ), #3691, .F. ) ;
#440 = DIRECTION ( 'NONE',  ( 0.000000000000000000, 1.224646799147353207E-16, -1.000000000000000000 ) ) ;
#441 = DIRECTION ( 'NONE',  ( 1.000000000000000000, 0.000000000000000000, 0.000000000000000000 ) ) ;
#442 = AXIS2_PLACEMENT_3D ( 'NONE', #1630, #400, #2242 ) ;
#443 = AXIS2_PLACEMENT_3D ( 'NONE', #885, #2071, #3254 ) ;
#444 = AXIS2_PLACEMENT_3D ( 'NONE', #1397, #2583, #1222 ) ;
#445 = ORIENTED_EDGE ( 'NONE', *, *, #866, .T. ) ;
#446 = FACE_OUTER_BOUND ( 'NONE', #1984, .T. ) ;
#447 = VERTEX_POINT ( 'NONE', #1262 ) ;
#448 = CARTESIAN_POINT ( 'NONE',  ( 0.000000000000000000, 0.000000000000000000, -15.70000000000000284 ) ) ;
#449 = CIRCLE ( 'NONE', #3007, 3.799999999999999378 ) ;
#450 = AXIS2_PLACEMENT_3D ( 'NONE', #3093, #409, #1599 ) ;
#451 = AXIS2_PLACEMENT_3D ( 'NONE', #1088, #2312, #3462 ) ;
#452 = DIRECTION ( 'NONE',  ( -1.000000000000000000, 0.000000000000000000, 0.000000000000000000 ) ) ;
#453 = EDGE_LOOP ( 'NONE', ( #297, #1815, #2065, #876 ) ) ;
#454 = FACE_OUTER_BOUND ( 'NONE', #746, .T. ) ;
#455 = DIRECTION ( 'NONE',  ( -1.000000000000000000, -0.000000000000000000, -0.000000000000000000 ) ) ;
#456 = FACE_OUTER_BOUND ( 'NONE', #836, .T. ) ;
#457 = EDGE_LOOP ( 'NONE', ( #3256, #3221, #3322, #30 ) ) ;
#458 = ORIENTED_EDGE ( 'NONE', *, *, #1532, .F. ) ;
#459 = CARTESIAN_POINT ( 'NONE',  ( 1.300000000000000044, -0.7216878364870319418, 1.249999999999999778 ) ) ;
#460 =( NAMED_UNIT ( * ) PLANE_ANGLE_UNIT ( ) SI_UNIT ( $, .RADIAN. ) );
#461 = EDGE_CURVE ( 'NONE', #2373, #2385, #1905, .T. ) ;
#462 = PRESENTATION_LAYER_ASSIGNMENT (  '', '', ( #3820 ) ) ;
#463 = AXIS2_PLACEMENT_3D ( 'NONE', #3102, #1058, #3695 ) ;
#464 = UNCERTAINTY_MEASURE_WITH_UNIT (LENGTH_MEASURE( 1.000000000000000082E-05 ), #2003, 'distance_accuracy_value', 'NONE');
#465 = VERTEX_POINT ( 'NONE', #3634 ) ;
#466 = CONTEXT_DEPENDENT_SHAPE_REPRESENTATION ( #2223, #3094 ) ;
#467 = ADVANCED_FACE ( 'NONE', ( #1337 ), #1299, .T. ) ;
#468 = STYLED_ITEM ( 'NONE', ( #939 ), #3116 ) ;
#469 = AXIS2_PLACEMENT_3D ( 'NONE', #940, #1573, #3367 ) ;
#470 = CARTESIAN_POINT ( 'NONE',  ( 1.820000000000000062, 0.000000000000000000, 0.000000000000000000 ) ) ;
#471 = DIRECTION ( 'NONE',  ( -1.000000000000000000, 0.000000000000000000, 0.000000000000000000 ) ) ;
#472 = CIRCLE ( 'NONE', #1713, 1.999999999999999112 ) ;
#473 = ORIENTED_EDGE ( 'NONE', *, *, #3077, .F. ) ;
#474 = CARTESIAN_POINT ( 'NONE',  ( 1.300000000000000044, 0.7216878364870329410, -1.250000000000000000 ) ) ;
#475 = EDGE_LOOP ( 'NONE', ( #2661, #3268, #2052, #1054 ) ) ;
#476 = CARTESIAN_POINT ( 'NONE',  ( 1.300000000000000044, 1.443375672974065216, 7.017607234860990640E-28 ) ) ;
#477 = PRODUCT_DEFINITION_CONTEXT ( 'detailed design', #626, 'design' ) ;
#478 = FACE_OUTER_BOUND ( 'NONE', #890, .T. ) ;
#479 = ORIENTED_EDGE ( 'NONE', *, *, #638, .F. ) ;
#480 = DIRECTION ( 'NONE',  ( 0.000000000000000000, -1.000000000000000000, 0.000000000000000000 ) ) ;
#481 = DIRECTION ( 'NONE',  ( 0.000000000000000000, 0.000000000000000000, 1.000000000000000000 ) ) ;
#482 = EDGE_CURVE ( 'NONE', #2228, #2253, #413, .T. ) ;
#483 = ORIENTED_EDGE ( 'NONE', *, *, #3700, .T. ) ;
#484 = FACE_OUTER_BOUND ( 'NONE', #2820, .T. ) ;
#485 = DIRECTION ( 'NONE',  ( -0.000000000000000000, -0.000000000000000000, -1.000000000000000000 ) ) ;
#486 = EDGE_CURVE ( 'NONE', #1598, #2646, #2955, .T. ) ;
#487 = CARTESIAN_POINT ( 'NONE',  ( 3.799999999999999378, 4.653657836759941744E-16, 0.000000000000000000 ) ) ;
#488 = CARTESIAN_POINT ( 'NONE',  ( 0.000000000000000000, 0.000000000000000000, 0.000000000000000000 ) ) ;
#489 = ORIENTED_EDGE ( 'NONE', *, *, #2922, .F. ) ;
#490 = LINE ( 'NONE', #3484, #318 ) ;
#491 = ORIENTED_EDGE ( 'NONE', *, *, #1833, .T. ) ;
#492 = ADVANCED_FACE ( 'NONE', ( #3403 ), #2773, .T. ) ;
#493 = DIRECTION ( 'NONE',  ( 1.000000000000000000, 0.000000000000000000, 0.000000000000000000 ) ) ;
#494 = VERTEX_POINT ( 'NONE', #975 ) ;
#495 = DIRECTION ( 'NONE',  ( -0.000000000000000000, -0.000000000000000000, -1.000000000000000000 ) ) ;
#496 = CARTESIAN_POINT ( 'NONE',  ( 0.000000000000000000, 0.000000000000000000, 0.000000000000000000 ) ) ;
#497 = ORIENTED_EDGE ( 'NONE', *, *, #2033, .T. ) ;
#498 = DIRECTION ( 'NONE',  ( -1.000000000000000000, 0.000000000000000000, 0.000000000000000000 ) ) ;
#499 = CARTESIAN_POINT ( 'NONE',  ( 0.000000000000000000, 0.000000000000000000, -8.000000000000000000 ) ) ;
#500 = FILL_AREA_STYLE_COLOUR ( '', #2522 ) ;
#501 = CARTESIAN_POINT ( 'NONE',  ( 0.000000000000000000, -0.000000000000000000, 0.000000000000000000 ) ) ;
#502 = CARTESIAN_POINT ( 'NONE',  ( 28.92857142857272379, 7.945926950454914817, 5.000000000000000000 ) ) ;
#503 = ORIENTED_EDGE ( 'NONE', *, *, #2320, .F. ) ;
#504 = AXIS2_PLACEMENT_3D ( 'NONE', #2399, #1248, #996 ) ;
#505 = CARTESIAN_POINT ( 'NONE',  ( -82.50000000000000000, -19.84313483298442904, 0.000000000000000000 ) ) ;
#506 = EDGE_LOOP ( 'NONE', ( #2013, #1714, #3610, #3275 ) ) ;
#507 = EDGE_CURVE ( 'NONE', #620, #2556, #2157, .T. ) ;
#508 = MECHANICAL_DESIGN_GEOMETRIC_PRESENTATION_REPRESENTATION (  '', ( #1945 ), #1017 ) ;
#509 = COLOUR_RGB ( '',1.000000000000000000, 0.9490196078431372140, 0.9098039215686274384 ) ;
#510 = DIRECTION ( 'NONE',  ( -0.000000000000000000, -0.000000000000000000, -1.000000000000000000 ) ) ;
#511 = VERTEX_POINT ( 'NONE', #694 ) ;
#512 = LINE ( 'NONE', #1143, #279 ) ;
#513 = VECTOR ( 'NONE', #2474, 1000.000000000000000 ) ;
#514 = AXIS2_PLACEMENT_3D ( 'NONE', #1091, #878, #2301 ) ;
#515 = DIRECTION ( 'NONE',  ( 0.000000000000000000, -1.000000000000000000, 0.000000000000000000 ) ) ;
#516 = EDGE_CURVE ( 'NONE', #3615, #1351, #3346, .T. ) ;
#517 = EDGE_CURVE ( 'NONE', #1737, #494, #1548, .T. ) ;
#518 = CIRCLE ( 'NONE', #3813, 4.324969328314201888 ) ;
#519 = ORIENTED_EDGE ( 'NONE', *, *, #3486, .T. ) ;
#520 = CARTESIAN_POINT ( 'NONE',  ( 0.000000000000000000, 0.000000000000000000, 0.000000000000000000 ) ) ;
#521 = DIRECTION ( 'NONE',  ( -1.000000000000000000, 0.000000000000000000, 0.000000000000000000 ) ) ;
#522 = DIRECTION ( 'NONE',  ( 1.000000000000000000, 0.000000000000000000, 0.000000000000000000 ) ) ;
#523 = VECTOR ( 'NONE', #690, 1000.000000000000114 ) ;
#524 = ORIENTED_EDGE ( 'NONE', *, *, #3730, .F. ) ;
#525 = DIRECTION ( 'NONE',  ( 0.000000000000000000, 0.000000000000000000, -1.000000000000000000 ) ) ;
#526 = DIRECTION ( 'NONE',  ( 0.000000000000000000, 0.000000000000000000, 1.000000000000000000 ) ) ;
#527 = AXIS2_PLACEMENT_3D ( 'NONE', #922, #2066, #1791 ) ;
#528 = AXIS2_PLACEMENT_3D ( 'NONE', #2164, #3336, #2490 ) ;
#529 = EDGE_LOOP ( 'NONE', ( #1931, #3571, #1260, #616, #3835 ) ) ;
#530 = DIRECTION ( 'NONE',  ( -1.000000000000000000, 0.000000000000000000, -0.000000000000000000 ) ) ;
#531 = EDGE_LOOP ( 'NONE', ( #830, #1241, #942, #1732 ) ) ;
#532 = AXIS2_PLACEMENT_3D ( 'NONE', #3160, #1989, #3703 ) ;
#533 = PRODUCT_DEFINITION_FORMATION_WITH_SPECIFIED_SOURCE ( 'ANY', '', #1906, .NOT_KNOWN. ) ;
#534 = DIRECTION ( 'NONE',  ( 0.6221102074731698073, 0.4753501651576230724, -0.6221102074731695852 ) ) ;
#535 = VERTEX_POINT ( 'NONE', #2466 ) ;
#536 = CARTESIAN_POINT ( 'NONE',  ( -4.375000000000001776, -34.72548595772274638, -30.00000000000000000 ) ) ;
#537 = PRODUCT_DEFINITION ( 'UNKNOWN', '', #3334, #2544 ) ;
#538 = DIRECTION ( 'NONE',  ( 0.000000000000000000, 0.000000000000000000, 1.000000000000000000 ) ) ;
#539 = ORIENTED_EDGE ( 'NONE', *, *, #1536, .T. ) ;
#540 = DIRECTION ( 'NONE',  ( -0.000000000000000000, -0.000000000000000000, -1.000000000000000000 ) ) ;
#541 = DIRECTION ( 'NONE',  ( -0.000000000000000000, -0.000000000000000000, 1.000000000000000000 ) ) ;
#542 = DIRECTION ( 'NONE',  ( 1.000000000000000000, 0.000000000000000000, 0.000000000000000000 ) ) ;
#543 = ORIENTED_EDGE ( 'NONE', *, *, #1379, .T. ) ;
#544 = CARTESIAN_POINT ( 'NONE',  ( 0.000000000000000000, 0.000000000000000000, -8.000000000000000000 ) ) ;
#545 = FILL_AREA_STYLE ('',( #2106 ) ) ;
#546 = EDGE_CURVE ( 'NONE', #671, #2369, #590, .T. ) ;
#547 = CARTESIAN_POINT ( 'NONE',  ( 0.000000000000000000, 0.000000000000000000, 0.000000000000000000 ) ) ;
#548 = ORIENTED_EDGE ( 'NONE', *, *, #1378, .T. ) ;
#549 = EDGE_CURVE ( 'NONE', #1148, #2170, #2172, .T. ) ;
#550 = ORIENTED_EDGE ( 'NONE', *, *, #2872, .F. ) ;
#551 = FACE_OUTER_BOUND ( 'NONE', #1433, .T. ) ;
#552 = ORIENTED_EDGE ( 'NONE', *, *, #835, .F. ) ;
#553 = DIRECTION ( 'NONE',  ( 0.000000000000000000, -1.000000000000000000, 0.000000000000000000 ) ) ;
#554 = CARTESIAN_POINT ( 'NONE',  ( 2.200000000000000622, 0.000000000000000000, 0.000000000000000000 ) ) ;
#555 = ADVANCED_FACE ( 'NONE', ( #1010 ), #2255, .T. ) ;
#556 = SHAPE_REPRESENTATION ( 'socket button head screw_iso_ISO 7380 - M4 x 10 - 10N', ( #2207 ), #1040 ) ;
#557 = SHAPE_DEFINITION_REPRESENTATION ( #2389, #681 ) ;
#558 = ORIENTED_EDGE ( 'NONE', *, *, #2721, .F. ) ;
#559 = DIRECTION ( 'NONE',  ( -1.000000000000000000, -0.000000000000000000, -0.000000000000000000 ) ) ;
#560 = CARTESIAN_POINT ( 'NONE',  ( 11.80999999999999872, 0.000000000000000000, 1.999999999999999556 ) ) ;
#561 = EDGE_CURVE ( 'NONE', #2858, #2217, #1358, .T. ) ;
#562 = EDGE_CURVE ( 'NONE', #1255, #1889, #331, .T. ) ;
#563 = EDGE_LOOP ( 'NONE', ( #2991, #2903, #3738, #178 ) ) ;
#564 = EDGE_CURVE ( 'NONE', #1187, #929, #2020, .T. ) ;
#565 = DIRECTION ( 'NONE',  ( -1.000000000000000000, 0.000000000000000000, -0.000000000000000000 ) ) ;
#566 = EDGE_CURVE ( 'NONE', #3824, #3666, #844, .T. ) ;
#567 = EDGE_CURVE ( 'NONE', #2170, #2092, #1335, .T. ) ;
#568 = DIRECTION ( 'NONE',  ( -0.000000000000000000, 0.5000000000000000000, 0.8660254037844385966 ) ) ;
#569 = ORIENTED_EDGE ( 'NONE', *, *, #3600, .T. ) ;
#570 = CIRCLE ( 'NONE', #374, 3.799999999999999378 ) ;
#571 = ORIENTED_EDGE ( 'NONE', *, *, #2102, .F. ) ;
#572 =( NAMED_UNIT ( * ) PLANE_ANGLE_UNIT ( ) SI_UNIT ( $, .RADIAN. ) );
#573 = VERTEX_POINT ( 'NONE', #1808 ) ;
#574 = CARTESIAN_POINT ( 'NONE',  ( 0.000000000000000000, 0.000000000000000000, -14.99999999999999645 ) ) ;
#575 = FACE_BOUND ( 'NONE', #2885, .T. ) ;
#576 =( GEOMETRIC_REPRESENTATION_CONTEXT ( 3 ) GLOBAL_UNCERTAINTY_ASSIGNED_CONTEXT ( ( #464 ) ) GLOBAL_UNIT_ASSIGNED_CONTEXT ( ( #2003, #2025, #3522 ) ) REPRESENTATION_CONTEXT ( 'NONE', 'WORKASPACE' ) );
#577 = AXIS2_PLACEMENT_3D ( 'NONE', #710, #3339, #1868 ) ;
#578 = VECTOR ( 'NONE', #2424, 1000.000000000000000 ) ;
#579 = ORIENTED_EDGE ( 'NONE', *, *, #2275, .F. ) ;
#580 = PLANE ( 'NONE',  #2653 ) ;
#581 = CARTESIAN_POINT ( 'NONE',  ( 0.000000000000000000, -0.000000000000000000, 0.000000000000000000 ) ) ;
#582 = CARTESIAN_POINT ( 'NONE',  ( -41.00013885766087185, -69.84991647008799021, 1.802946974245779548E-15 ) ) ;
#583 = PRODUCT_DEFINITION ( 'UNKNOWN', '', #533, #199 ) ;
#584 = AXIS2_PLACEMENT_3D ( 'NONE', #1486, #55, #3633 ) ;
#585 = ORIENTED_EDGE ( 'NONE', *, *, #317, .T. ) ;
#586 = CARTESIAN_POINT ( 'NONE',  ( 0.000000000000000000, 0.7216878364870329410, -1.250000000000000000 ) ) ;
#587 = VECTOR ( 'NONE', #2366, 1000.000000000000114 ) ;
#588 = CARTESIAN_POINT ( 'NONE',  ( 1.300000000000000044, -1.443375672974064328, 1.278502688459867223E-18 ) ) ;
#589 = EDGE_CURVE ( 'NONE', #3785, #3235, #2707, .T. ) ;
#590 = CIRCLE ( 'NONE', #2764, 1.325000000000000622 ) ;
#591 = CARTESIAN_POINT ( 'NONE',  ( 1.300000000000000044, 0.7216878364870328300, 1.249999999999999778 ) ) ;
#592 = ORIENTED_EDGE ( 'NONE', *, *, #78, .T. ) ;
#593 = CIRCLE ( 'NONE', #2088, 4.500000000000000888 ) ;
#594 = ORIENTED_EDGE ( 'NONE', *, *, #638, .T. ) ;
#595 = CARTESIAN_POINT ( 'NONE',  ( -80.00000000000000000, 0.000000000000000000, -4.999999999999997335 ) ) ;
#596 = ORIENTED_EDGE ( 'NONE', *, *, #300, .T. ) ;
#597 = PRESENTATION_LAYER_ASSIGNMENT (  '', '', ( #785 ) ) ;
#598 = AXIS2_PLACEMENT_3D ( 'NONE', #3513, #255, #2913 ) ;
#599 = CARTESIAN_POINT ( 'NONE',  ( -1.999999999999999112, 0.000000000000000000, -20.00000000000000000 ) ) ;
#600 = CIRCLE ( 'NONE', #3082, 1.999999999999998224 ) ;
#601 = ORIENTED_EDGE ( 'NONE', *, *, #3693, .F. ) ;
#602 = LINE ( 'NONE', #2115, #383 ) ;
#603 = LINE ( 'NONE', #2116, #3452 ) ;
#604 = EDGE_CURVE ( 'NONE', #964, #511, #1830, .T. ) ;
#605 = VERTEX_POINT ( 'NONE', #606 ) ;
#606 = CARTESIAN_POINT ( 'NONE',  ( 2.200000000000000622, 0.000000000000000000, 2.199999999999999289 ) ) ;
#607 = DIRECTION ( 'NONE',  ( 1.000000000000000000, 0.000000000000000000, -0.000000000000000000 ) ) ;
#608 = ADVANCED_FACE ( 'NONE', ( #1475 ), #848, .T. ) ;
#609 = DIRECTION ( 'NONE',  ( -0.000000000000000000, -0.000000000000000000, -1.000000000000000000 ) ) ;
#610 = ORIENTED_EDGE ( 'NONE', *, *, #809, .F. ) ;
#611 = VERTEX_POINT ( 'NONE', #2374 ) ;
#613 = ORIENTED_EDGE ( 'NONE', *, *, #1657, .T. ) ;
#612 = EDGE_CURVE ( 'NONE', #2092, #1136, #2029, .T. ) ;
#614 = FACE_OUTER_BOUND ( 'NONE', #2550, .T. ) ;
#615 = CLOSED_SHELL ( 'NONE', ( #99, #3472, #2462, #648 ) ) ;
#616 = ORIENTED_EDGE ( 'NONE', *, *, #507, .F. ) ;
#617 = DIRECTION ( 'NONE',  ( -0.000000000000000000, -0.000000000000000000, -1.000000000000000000 ) ) ;
#618 = DIRECTION ( 'NONE',  ( -1.224646799147353207E-16, 1.000000000000000000, 0.000000000000000000 ) ) ;
#619 = DIRECTION ( 'NONE',  ( -0.5873034230612221851, -0.8093668446758681689, 0.000000000000000000 ) ) ;
#620 = VERTEX_POINT ( 'NONE', #956 ) ;
#621 = CARTESIAN_POINT ( 'NONE',  ( 1.300000000000000044, -0.7216878364870318308, -1.250000000000000000 ) ) ;
#622 = FACE_OUTER_BOUND ( 'NONE', #2781, .T. ) ;
#623 = DIRECTION ( 'NONE',  ( -0.000000000000000000, -0.000000000000000000, -1.000000000000000000 ) ) ;
#624 = CARTESIAN_POINT ( 'NONE',  ( 1.300000000000000044, 1.082531754730548856, -0.6250000000000002220 ) ) ;
#625 = PRODUCT_DEFINITION_SHAPE ( 'NONE', 'NONE',  #3841 ) ;
#626 = APPLICATION_CONTEXT ( 'automotive_design' ) ;
#627 = B_SPLINE_CURVE_WITH_KNOTS ( 'NONE', 3,
 ( #187, #1692, #2876, #2337 ),
 .UNSPECIFIED., .F., .F.,
 ( 4, 4 ),
 ( 0.000000000000000000, 1.000000000000000000 ),
 .UNSPECIFIED. ) ;
#628 = ORIENTED_EDGE ( 'NONE', *, *, #206, .F. ) ;
#629 = CARTESIAN_POINT ( 'NONE',  ( 0.000000000000000000, 0.000000000000000000, -20.00000000000000000 ) ) ;
#630 = ORIENTED_EDGE ( 'NONE', *, *, #750, .T. ) ;
#631 = FACE_OUTER_BOUND ( 'NONE', #28, .T. ) ;
#632 = VECTOR ( 'NONE', #1734, 1000.000000000000000 ) ;
#633 = ORIENTED_EDGE ( 'NONE', *, *, #1532, .T. ) ;
#634 = CYLINDRICAL_SURFACE ( 'NONE', #3503, 1.999999999999999112 ) ;
#635 = DIRECTION ( 'NONE',  ( 1.000000000000000000, 0.000000000000000000, 0.000000000000000000 ) ) ;
#636 = AXIS2_PLACEMENT_3D ( 'NONE', #1943, #2917, #1452 ) ;
#637 =( NAMED_UNIT ( * ) SI_UNIT ( $, .STERADIAN. ) SOLID_ANGLE_UNIT ( ) );
#638 = EDGE_CURVE ( 'NONE', #15, #2226, #783, .T. ) ;
#639 = VECTOR ( 'NONE', #2886, 1000.000000000000000 ) ;
#640 = AXIS2_PLACEMENT_3D ( 'NONE', #2895, #225, #538 ) ;
#641 = DIRECTION ( 'NONE',  ( -0.9921567416492214075, 0.1250000000000000555, 0.000000000000000000 ) ) ;
#642 = CARTESIAN_POINT ( 'NONE',  ( 29.64285714285758999, 5.345441766669614125, 3.727272727272256336 ) ) ;
#643 = AXIS2_PLACEMENT_3D ( 'NONE', #1477, #2403, #9 ) ;
#644 = AXIS2_PLACEMENT_3D ( 'NONE', #2215, #2193, #3654 ) ;
#645 = AXIS2_PLACEMENT_3D ( 'NONE', #68, #3596, #933 ) ;
#646 = DIRECTION ( 'NONE',  ( -1.000000000000000000, -0.000000000000000000, -0.000000000000000000 ) ) ;
#647 = DIRECTION ( 'NONE',  ( -1.000000000000000000, 0.000000000000000000, 0.000000000000000000 ) ) ;
#648 = ADVANCED_FACE ( 'NONE', ( #1170 ), #1153, .T. ) ;
#649 = ORIENTED_EDGE ( 'NONE', *, *, #2423, .F. ) ;
#650 = DIRECTION ( 'NONE',  ( 0.000000000000000000, 0.000000000000000000, 1.000000000000000000 ) ) ;
#651 = ORIENTED_EDGE ( 'NONE', *, *, #3049, .T. ) ;
#652 = DIRECTION ( 'NONE',  ( 1.000000000000000000, 0.000000000000000000, 0.000000000000000000 ) ) ;
#653 = PRODUCT_RELATED_PRODUCT_CATEGORY ( 'part', '', ( #3612 ) ) ;
#654 = MECHANICAL_DESIGN_GEOMETRIC_PRESENTATION_REPRESENTATION (  '', ( #785 ), #2832 ) ;
#655 = EDGE_LOOP ( 'NONE', ( #3357, #2286, #1960, #1641, #907, #1356, #3483, #1912 ) ) ;
#656 = DIRECTION ( 'NONE',  ( 0.000000000000000000, 0.000000000000000000, 1.000000000000000000 ) ) ;
#657 = CARTESIAN_POINT ( 'NONE',  ( -90.00000000000000000, 0.000000000000000000, -30.00000000000000000 ) ) ;
#658 = LINE ( 'NONE', #1244, #2009 ) ;
#659 = VECTOR ( 'NONE', #728, 1000.000000000000114 ) ;
#660 = UNCERTAINTY_MEASURE_WITH_UNIT (LENGTH_MEASURE( 1.000000000000000082E-05 ), #3741, 'distance_accuracy_value', 'NONE');
#661 = DIRECTION ( 'NONE',  ( -1.000000000000000000, -0.000000000000000000, -0.000000000000000000 ) ) ;
#662 = CARTESIAN_POINT ( 'NONE',  ( -80.00000000000000000, 0.000000000000000000, -30.00000000000000000 ) ) ;
#663 =( NAMED_UNIT ( * ) SI_UNIT ( $, .STERADIAN. ) SOLID_ANGLE_UNIT ( ) );
#664 = AXIS2_PLACEMENT_3D ( 'NONE', #2506, #2533, #3696 ) ;
#665 = EDGE_CURVE ( 'NONE', #3091, #3418, #215, .T. ) ;
#666 = CARTESIAN_POINT ( 'NONE',  ( 1.300000000000000044, -1.082531754730548190, 0.6250000000000002220 ) ) ;
#667 = EDGE_CURVE ( 'NONE', #1, #283, #3269, .T. ) ;
#668 = DIRECTION ( 'NONE',  ( -0.000000000000000000, -0.000000000000000000, -1.000000000000000000 ) ) ;
#669 = ORIENTED_EDGE ( 'NONE', *, *, #2050, .F. ) ;
#670 = DIRECTION ( 'NONE',  ( -0.1250000000000000555, -0.9921567416492214075, 0.000000000000000000 ) ) ;
#671 = VERTEX_POINT ( 'NONE', #3621 ) ;
#672 = FACE_OUTER_BOUND ( 'NONE', #3258, .T. ) ;
#673 = VERTEX_POINT ( 'NONE', #1773 ) ;
#674 = DIRECTION ( 'NONE',  ( 0.8571673007021117785, 1.049727191138617956E-16, -0.5150380749100550437 ) ) ;
#675 = CARTESIAN_POINT ( 'NONE',  ( -3.750000000000001776, -29.76470224947664178, -30.00000000000000000 ) ) ;
#676 = FILL_AREA_STYLE ('',( #3598 ) ) ;
#677 = CARTESIAN_POINT ( 'NONE',  ( 1.300000000000000044, -0.7216878364870317197, 1.250000000000000000 ) ) ;
#678 = ADVANCED_FACE ( 'NONE', ( #302 ), #2688, .F. ) ;
#679 = PLANE ( 'NONE',  #2123 ) ;
#680 =( LENGTH_UNIT ( ) NAMED_UNIT ( * ) SI_UNIT ( .MILLI., .METRE. ) );
#681 = SHAPE_REPRESENTATION ( 'MAS-190', ( #3395, #2524, #402, #1340, #2585, #912, #1223, #1527, #1722 ), #2902 ) ;
#682 = DIRECTION ( 'NONE',  ( -1.000000000000000000, 0.000000000000000000, 0.000000000000000000 ) ) ;
#683 = LINE ( 'NONE', #1271, #2694 ) ;
#684 = EDGE_CURVE ( 'NONE', #1516, #929, #1247, .T. ) ;
#685 = ADVANCED_FACE ( 'NONE', ( #1209 ), #2138, .T. ) ;
#686 = ORIENTED_EDGE ( 'NONE', *, *, #2064, .F. ) ;
#687 = DIRECTION ( 'NONE',  ( -1.000000000000000000, 0.000000000000000000, -0.000000000000000000 ) ) ;
#688 = VERTEX_POINT ( 'NONE', #265 ) ;
#689 = DIRECTION ( 'NONE',  ( 0.000000000000000000, 0.000000000000000000, 1.000000000000000000 ) ) ;
#690 = DIRECTION ( 'NONE',  ( -0.000000000000000000, -0.5000000000000002220, 0.8660254037844384856 ) ) ;
#691 = VERTEX_POINT ( 'NONE', #1455 ) ;
#692 = CARTESIAN_POINT ( 'NONE',  ( 1.300000000000000044, -0.7216878364870319418, 1.249999999999999778 ) ) ;
#693 = MANIFOLD_SOLID_BREP ( 'Base-Extrude', #871 ) ;
#694 = CARTESIAN_POINT ( 'NONE',  ( 0.000000000000000000, 0.7216878364870329410, -1.250000000000000000 ) ) ;
#695 = LINE ( 'NONE', #2173, #833 ) ;
#696 = AXIS2_PLACEMENT_3D ( 'NONE', #375, #3331, #59 ) ;
#697 = CARTESIAN_POINT ( 'NONE',  ( 0.000000000000000000, 0.000000000000000000, 0.000000000000000000 ) ) ;
#698 = VERTEX_POINT ( 'NONE', #1568 ) ;
#699 = DIRECTION ( 'NONE',  ( 1.000000000000000000, 0.000000000000000000, 0.000000000000000000 ) ) ;
#700 = SHAPE_REPRESENTATION_RELATIONSHIP ( 'NONE' , 'NONE' ,  #2152, #3116 ) ;
#701 = AXIS2_PLACEMENT_3D ( 'NONE', #3803, #2930, #772 ) ;
#702 = VECTOR ( 'NONE', #3081, 1000.000000000000227 ) ;
#703 = PRESENTATION_LAYER_ASSIGNMENT (  '', '', ( #1945 ) ) ;
#704 = AXIS2_PLACEMENT_3D ( 'NONE', #430, #1338, #1604 ) ;
#705 = DIRECTION ( 'NONE',  ( 0.000000000000000000, 1.224646799147353207E-16, -1.000000000000000000 ) ) ;
#706 = CARTESIAN_POINT ( 'NONE',  ( -3.749999999999998224, -29.76470224947664533, 0.000000000000000000 ) ) ;
#707 = EDGE_CURVE ( 'NONE', #1234, #1780, #2652, .T. ) ;
#708 = VECTOR ( 'NONE', #3356, 999.9999999999998863 ) ;
#709 = ORIENTED_EDGE ( 'NONE', *, *, #3416, .F. ) ;
#710 = CARTESIAN_POINT ( 'NONE',  ( -78.00000000000000000, 0.000000000000000000, 3.000000000000000000 ) ) ;
#711 = ORIENTED_EDGE ( 'NONE', *, *, #300, .F. ) ;
#712 = CIRCLE ( 'NONE', #1027, 1.899999999999999689 ) ;
#713 = DIRECTION ( 'NONE',  ( 1.000000000000000000, 0.000000000000000000, 0.000000000000000000 ) ) ;
#714 = DIRECTION ( 'NONE',  ( -1.000000000000000000, -0.000000000000000000, -0.000000000000000000 ) ) ;
#715 = VERTEX_POINT ( 'NONE', #2469 ) ;
#716 = DIRECTION ( 'NONE',  ( -0.000000000000000000, -1.000000000000000000, -0.000000000000000000 ) ) ;
#717 = DIRECTION ( 'NONE',  ( 0.000000000000000000, 0.000000000000000000, -1.000000000000000000 ) ) ;
#718 = CYLINDRICAL_SURFACE ( 'NONE', #1081, 3.799999999999999378 ) ;
#719 = EDGE_CURVE ( 'NONE', #2633, #964, #91, .T. ) ;
#720 = AXIS2_PLACEMENT_3D ( 'NONE', #176, #788, #1721 ) ;
#721 = AXIS2_PLACEMENT_3D ( 'NONE', #122, #2532, #1880 ) ;
#722 = DIRECTION ( 'NONE',  ( 1.000000000000000000, 0.000000000000000000, 0.000000000000000000 ) ) ;
#723 = ORIENTED_EDGE ( 'NONE', *, *, #612, .T. ) ;
#724 = DIRECTION ( 'NONE',  ( 1.000000000000000000, 0.000000000000000000, 0.000000000000000000 ) ) ;
#725 = SURFACE_STYLE_USAGE ( .BOTH. , #997 ) ;
#726 = VECTOR ( 'NONE', #1249, 1000.000000000000000 ) ;
#727 = EDGE_CURVE ( 'NONE', #80, #3822, #2957, .T. ) ;
#728 = DIRECTION ( 'NONE',  ( -0.000000000000000000, -0.5000000000000002220, 0.8660254037844384856 ) ) ;
#729 = CARTESIAN_POINT ( 'NONE',  ( 23.82500000000000284, 2.917720998968569322E-15, 0.000000000000000000 ) ) ;
#730 = ORIENTED_EDGE ( 'NONE', *, *, #2175, .F. ) ;
#731 = CARTESIAN_POINT ( 'NONE',  ( 0.000000000000000000, 0.000000000000000000, 0.000000000000000000 ) ) ;
#732 = ORIENTED_EDGE ( 'NONE', *, *, #3728, .T. ) ;
#733 = DIRECTION ( 'NONE',  ( -1.000000000000000000, 0.000000000000000000, 0.000000000000000000 ) ) ;
#734 = EDGE_CURVE ( 'NONE', #916, #926, #1606, .T. ) ;
#735 = DIRECTION ( 'NONE',  ( 1.000000000000000000, 0.000000000000000000, 0.000000000000000000 ) ) ;
#736 = EDGE_LOOP ( 'NONE', ( #3178, #3153, #1073, #2475, #172 ) ) ;
#737 = CARTESIAN_POINT ( 'NONE',  ( 1.820000000000000062, 0.000000000000000000, 0.000000000000000000 ) ) ;
#738 = CARTESIAN_POINT ( 'NONE',  ( 0.000000000000000000, -0.7216878364870317197, 1.250000000000000000 ) ) ;
#739 = DIRECTION ( 'NONE',  ( -1.000000000000000000, -0.000000000000000000, -0.000000000000000000 ) ) ;
#740 = EDGE_CURVE ( 'NONE', #1954, #1234, #2219, .T. ) ;
#741 =( LENGTH_UNIT ( ) NAMED_UNIT ( * ) SI_UNIT ( .MILLI., .METRE. ) );
#742 = VERTEX_POINT ( 'NONE', #3385 ) ;
#743 = CARTESIAN_POINT ( 'NONE',  ( -80.00000000000000000, 0.000000000000000000, -5.000000000000000000 ) ) ;
#744 = CARTESIAN_POINT ( 'NONE',  ( 1.820000000000000062, 0.000000000000000000, 3.799999999999999378 ) ) ;
#745 = DIRECTION ( 'NONE',  ( -0.000000000000000000, 1.000000000000000000, 1.224646799147353207E-16 ) ) ;
#746 = EDGE_LOOP ( 'NONE', ( #610, #2576 ) ) ;
#747 =( LENGTH_UNIT ( ) NAMED_UNIT ( * ) SI_UNIT ( .MILLI., .METRE. ) );
#748 = VERTEX_POINT ( 'NONE', #1266 ) ;
#749 = DIRECTION ( 'NONE',  ( -0.000000000000000000, 0.5000000000000002220, -0.8660254037844384856 ) ) ;
#750 = EDGE_CURVE ( 'NONE', #2723, #2369, #1277, .T. ) ;
#751 = UNCERTAINTY_MEASURE_WITH_UNIT (LENGTH_MEASURE( 1.000000000000000082E-05 ), #1401, 'distance_accuracy_value', 'NONE');
#752 = DIRECTION ( 'NONE',  ( 0.9921567416492214075, 0.1250000000000001388, 0.000000000000000000 ) ) ;
#753 = ORIENTED_EDGE ( 'NONE', *, *, #1610, .F. ) ;
#754 = CARTESIAN_POINT ( 'NONE',  ( 34.99999999999999289, 0.000000000000000000, 4.999999999999997335 ) ) ;
#755 = DIRECTION ( 'NONE',  ( 0.9921567416492215186, 0.1250000000000001665, 0.000000000000000000 ) ) ;
#756 = FACE_OUTER_BOUND ( 'NONE', #3199, .T. ) ;
#757 = VERTEX_POINT ( 'NONE', #1550 ) ;
#758 = VERTEX_POINT ( 'NONE', #107 ) ;
#759 = SPHERICAL_SURFACE ( 'NONE', #636, 4.324969328314201888 ) ;
#760 = AXIS2_PLACEMENT_3D ( 'NONE', #544, #883, #2067 ) ;
#761 = APPLICATION_PROTOCOL_DEFINITION ( 'draft international standard', 'automotive_design', 1998, #3415 ) ;
#762 = CARTESIAN_POINT ( 'NONE',  ( 3.885274725274725949, -4.336808689942017736E-16, 0.000000000000000000 ) ) ;
#763 = CIRCLE ( 'NONE', #1018, 34.99999999999999289 ) ;
#764 = AXIS2_PLACEMENT_3D ( 'NONE', #179, #3725, #2829 ) ;
#765 = CIRCLE ( 'NONE', #2944, 2.000000000000001776 ) ;
#766 = EDGE_LOOP ( 'NONE', ( #2477, #3283 ) ) ;
#767 = CARTESIAN_POINT ( 'NONE',  ( -1.649999999999999245, 0.000000000000000000, -20.00000000000000000 ) ) ;
#768 = EDGE_LOOP ( 'NONE', ( #336, #812, #1881, #3232, #2122 ) ) ;
#769 = PLANE ( 'NONE',  #2386 ) ;
#770 = AXIS2_PLACEMENT_3D ( 'NONE', #3342, #3320, #1841 ) ;
#771 = AXIS2_PLACEMENT_3D ( 'NONE', #1959, #2015, #3203 ) ;
#772 = DIRECTION ( 'NONE',  ( 0.000000000000000000, -1.224646799147353207E-16, 1.000000000000000000 ) ) ;
#773 = ORIENTED_EDGE ( 'NONE', *, *, #2847, .T. ) ;
#774 = CARTESIAN_POINT ( 'NONE',  ( -23.82500000000000284, 0.000000000000000000, 0.000000000000000000 ) ) ;
#775 = DIRECTION ( 'NONE',  ( 1.000000000000000000, 0.000000000000000000, 0.000000000000000000 ) ) ;
#776 = ADVANCED_FACE ( 'NONE', ( #1341 ), #3638, .F. ) ;
#777 = VECTOR ( 'NONE', #1283, 1000.000000000000000 ) ;
#778 = ORIENTED_EDGE ( 'NONE', *, *, #3778, .T. ) ;
#779 = DIRECTION ( 'NONE',  ( 1.000000000000000000, 0.000000000000000000, -0.000000000000000000 ) ) ;
#780 = CARTESIAN_POINT ( 'NONE',  ( -82.50000000000000000, 19.84313483298442193, 0.000000000000000000 ) ) ;
#781 = APPLICATION_CONTEXT ( 'automotive_design' ) ;
#782 = AXIS2_PLACEMENT_3D ( 'NONE', #1045, #3410, #1636 ) ;
#783 = CIRCLE ( 'NONE', #3389, 1.649999999999999911 ) ;
#784 = PRODUCT_CONTEXT ( 'NONE', #418, 'mechanical' ) ;
#785 = STYLED_ITEM ( 'NONE', ( #3425 ), #1526 ) ;
#786 = CIRCLE ( 'NONE', #469, 7.000000000000000000 ) ;
#787 = PLANE ( 'NONE',  #1344 ) ;
#788 = DIRECTION ( 'NONE',  ( 0.000000000000000000, 0.000000000000000000, 1.000000000000000000 ) ) ;
#789 = VECTOR ( 'NONE', #3057, 1000.000000000000114 ) ;
#790 = ORIENTED_EDGE ( 'NONE', *, *, #2754, .F. ) ;
#791 = ADVANCED_BREP_SHAPE_REPRESENTATION ( '', ( #1966, #2207 ), #968 ) ;
#792 = DIRECTION ( 'NONE',  ( 0.000000000000000000, 0.000000000000000000, 1.000000000000000000 ) ) ;
#793 = ORIENTED_EDGE ( 'NONE', *, *, #1047, .F. ) ;
#794 = PRODUCT_DEFINITION_CONTEXT ( 'detailed design', #1619, 'design' ) ;
#795 = DIRECTION ( 'NONE',  ( -1.000000000000000000, -0.000000000000000000, -0.000000000000000000 ) ) ;
#796 = EDGE_LOOP ( 'NONE', ( #3689, #2096 ) ) ;
#797 = DIRECTION ( 'NONE',  ( 0.000000000000000000, 0.000000000000000000, 1.000000000000000000 ) ) ;
#798 = DIRECTION ( 'NONE',  ( -0.000000000000000000, 0.5000000000000002220, -0.8660254037844384856 ) ) ;
#799 = ORIENTED_EDGE ( 'NONE', *, *, #2239, .T. ) ;
#800 = CARTESIAN_POINT ( 'NONE',  ( 9.809999999999998721, 0.000000000000000000, 1.999999999999999556 ) ) ;
#801 = CARTESIAN_POINT ( 'NONE',  ( 1.600000000000000089, 0.000000000000000000, 0.000000000000000000 ) ) ;
#802 = EDGE_CURVE ( 'NONE', #1148, #2036, #154, .T. ) ;
#803 = DIRECTION ( 'NONE',  ( 1.000000000000000000, 0.000000000000000000, 0.000000000000000000 ) ) ;
#804 = EDGE_CURVE ( 'NONE', #1813, #2443, #2339, .T. ) ;
#805 = ORIENTED_EDGE ( 'NONE', *, *, #3212, .T. ) ;
#806 = DIRECTION ( 'NONE',  ( -0.9921567416492214075, 0.1250000000000000555, 0.000000000000000000 ) ) ;
#807 = ORIENTED_EDGE ( 'NONE', *, *, #3136, .F. ) ;
#808 = EDGE_CURVE ( 'NONE', #283, #1408, #2240, .T. ) ;
#809 = EDGE_CURVE ( 'NONE', #385, #671, #35, .T. ) ;
#810 = TOROIDAL_SURFACE ( 'NONE', #1437, 2.899999999999999911, 0.8999999999999999112 ) ;
#811 = CARTESIAN_POINT ( 'NONE',  ( 1.600000000000000089, 0.000000000000000000, 2.700000000000000178 ) ) ;
#812 = ORIENTED_EDGE ( 'NONE', *, *, #1575, .T. ) ;
#813 = CYLINDRICAL_SURFACE ( 'NONE', #1460, 4.499999999999997335 ) ;
#814 = DIRECTION ( 'NONE',  ( 0.000000000000000000, 0.000000000000000000, 1.000000000000000000 ) ) ;
#815 = ORIENTED_EDGE ( 'NONE', *, *, #2560, .T. ) ;
#816 = CARTESIAN_POINT ( 'NONE',  ( 0.000000000000000000, 0.000000000000000000, -8.000000000000000000 ) ) ;
#817 =( NAMED_UNIT ( * ) SI_UNIT ( $, .STERADIAN. ) SOLID_ANGLE_UNIT ( ) );
#818 = VERTEX_POINT ( 'NONE', #398 ) ;
#819 = DIRECTION ( 'NONE',  ( 0.000000000000000000, 0.000000000000000000, 1.000000000000000000 ) ) ;
#820 = CARTESIAN_POINT ( 'NONE',  ( 0.000000000000000000, 0.000000000000000000, 0.000000000000000000 ) ) ;
#821 = VERTEX_POINT ( 'NONE', #3348 ) ;
#822 = VECTOR ( 'NONE', #1593, 999.9999999999998863 ) ;
#823 =( LENGTH_UNIT ( ) NAMED_UNIT ( * ) SI_UNIT ( .MILLI., .METRE. ) );
#824 = ORIENTED_EDGE ( 'NONE', *, *, #482, .F. ) ;
#825 = EDGE_CURVE ( 'NONE', #3629, #1478, #3262, .T. ) ;
#826 = CIRCLE ( 'NONE', #1320, 20.00000000000000355 ) ;
#827 = AXIS2_PLACEMENT_3D ( 'NONE', #1745, #2304, #2589 ) ;
#828 = UNCERTAINTY_MEASURE_WITH_UNIT (LENGTH_MEASURE( 1.000000000000000082E-05 ), #45, 'distance_accuracy_value', 'NONE');
#829 = DIRECTION ( 'NONE',  ( -1.000000000000000000, -0.000000000000000000, -0.000000000000000000 ) ) ;
#830 = ORIENTED_EDGE ( 'NONE', *, *, #809, .T. ) ;
#831 = FACE_OUTER_BOUND ( 'NONE', #3651, .T. ) ;
#832 = VECTOR ( 'NONE', #405, 1000.000000000000000 ) ;
#833 = VECTOR ( 'NONE', #739, 1000.000000000000000 ) ;
#834 = FACE_OUTER_BOUND ( 'NONE', #3097, .T. ) ;
#835 = EDGE_CURVE ( 'NONE', #929, #1729, #1301, .T. ) ;
#836 = EDGE_LOOP ( 'NONE', ( #1395, #5, #966, #3713, #3401, #3386 ) ) ;
#837 = CARTESIAN_POINT ( 'NONE',  ( -80.00000000000000000, 0.000000000000000000, 5.000000000000000000 ) ) ;
#838 = CARTESIAN_POINT ( 'NONE',  ( 0.000000000000000000, 0.000000000000000000, -30.00000000000000000 ) ) ;
#839 = CARTESIAN_POINT ( 'NONE',  ( 0.000000000000000000, 0.000000000000000000, 0.000000000000000000 ) ) ;
#840 = CIRCLE ( 'NONE', #3141, 0.8999999999999999112 ) ;
#841 = EDGE_LOOP ( 'NONE', ( #254, #990, #1674, #1273, #1658, #1329, #1704 ) ) ;
#842 = LINE ( 'NONE', #2086, #1695 ) ;
#843 = PRESENTATION_STYLE_ASSIGNMENT (( #2655 ) ) ;
#844 = CIRCLE ( 'NONE', #3019, 30.00000000000000000 ) ;
#845 = ADVANCED_FACE ( 'NONE', ( #3670 ), #1013, .T. ) ;
#846 = CIRCLE ( 'NONE', #782, 1.324999999999999734 ) ;
#847 = COLOUR_RGB ( '',1.000000000000000000, 0.9490196078431372140, 0.9098039215686274384 ) ;
#848 = CONICAL_SURFACE ( 'NONE', #1963, 1.610000000000000098, 0.7853981633974458365 ) ;
#849 = CYLINDRICAL_SURFACE ( 'NONE', #764, 5.000000000000004441 ) ;
#850 = ORIENTED_EDGE ( 'NONE', *, *, #2359, .T. ) ;
#851 = VECTOR ( 'NONE', #3438, 1000.000000000000000 ) ;
#852 = ORIENTED_EDGE ( 'NONE', *, *, #1811, .T. ) ;
#853 = PRODUCT_DEFINITION_FORMATION_WITH_SPECIFIED_SOURCE ( 'ANY', '', #3643, .NOT_KNOWN. ) ;
#854 = EDGE_CURVE ( 'NONE', #3666, #1351, #1907, .T. ) ;
#855 = EDGE_CURVE ( 'NONE', #1639, #1544, #2142, .T. ) ;
#856 = CARTESIAN_POINT ( 'NONE',  ( 0.000000000000000000, 0.000000000000000000, 0.000000000000000000 ) ) ;
#857 = ORIENTED_EDGE ( 'NONE', *, *, #1052, .T. ) ;
#858 = LINE ( 'NONE', #2300, #1159 ) ;
#859 = DIRECTION ( 'NONE',  ( 0.000000000000000000, -1.502314598737159031E-16, -1.000000000000000000 ) ) ;
#860 = ADVANCED_FACE ( 'NONE', ( #1357 ), #1602, .T. ) ;
#861 = ITEM_DEFINED_TRANSFORMATION ( 'NONE', 'NONE', #1340,  #2207 ) ;
#862 = ORIENTED_EDGE ( 'NONE', *, *, #1617, .F. ) ;
#863 = DIRECTION ( 'NONE',  ( -1.000000000000000000, 0.000000000000000000, 0.000000000000000000 ) ) ;
#864 = CARTESIAN_POINT ( 'NONE',  ( -85.36741282452705093, -22.33760634779116572, 4.999999999999999112 ) ) ;
#865 =( NAMED_UNIT ( * ) SI_UNIT ( $, .STERADIAN. ) SOLID_ANGLE_UNIT ( ) );
#866 = EDGE_CURVE ( 'NONE', #2558, #1368, #412, .T. ) ;
#867 = EDGE_CURVE ( 'NONE', #2247, #1784, #1858, .T. ) ;
#868 = VERTEX_POINT ( 'NONE', #2547 ) ;
#869 = LINE ( 'NONE', #2673, #2691 ) ;
#870 = CARTESIAN_POINT ( 'NONE',  ( 0.000000000000000000, 0.000000000000000000, 0.000000000000000000 ) ) ;
#871 = CLOSED_SHELL ( 'NONE', ( #2181, #2910, #1552, #3450, #2335, #2348 ) ) ;
#872 = LINE ( 'NONE', #3231, #2503 ) ;
#873 = ORIENTED_EDGE ( 'NONE', *, *, #2182, .T. ) ;
#874 = ORIENTED_EDGE ( 'NONE', *, *, #3658, .F. ) ;
#875 = DIRECTION ( 'NONE',  ( 1.000000000000000000, 0.000000000000000000, 0.000000000000000000 ) ) ;
#876 = ORIENTED_EDGE ( 'NONE', *, *, #1758, .T. ) ;
#877 = FACE_OUTER_BOUND ( 'NONE', #3535, .T. ) ;
#878 = DIRECTION ( 'NONE',  ( -0.000000000000000000, -0.000000000000000000, -1.000000000000000000 ) ) ;
#879 = ORIENTED_EDGE ( 'NONE', *, *, #3782, .F. ) ;
#880 = DIRECTION ( 'NONE',  ( -1.000000000000000000, -0.000000000000000000, -0.000000000000000000 ) ) ;
#881 = DIRECTION ( 'NONE',  ( -1.000000000000000000, -0.000000000000000000, -0.000000000000000000 ) ) ;
#882 = ORIENTED_EDGE ( 'NONE', *, *, #3649, .T. ) ;
#883 = DIRECTION ( 'NONE',  ( 0.000000000000000000, 0.000000000000000000, 1.000000000000000000 ) ) ;
#884 =( LENGTH_UNIT ( ) NAMED_UNIT ( * ) SI_UNIT ( .MILLI., .METRE. ) );
#885 = CARTESIAN_POINT ( 'NONE',  ( 0.000000000000000000, 0.000000000000000000, 0.000000000000000000 ) ) ;
#886 = ORIENTED_EDGE ( 'NONE', *, *, #3729, .T. ) ;
#887 = CIRCLE ( 'NONE', #2621, 5.000000000000004441 ) ;
#888 = ORIENTED_EDGE ( 'NONE', *, *, #808, .T. ) ;
#889 = CARTESIAN_POINT ( 'NONE',  ( 12.20000000000000107, 2.210487472460972205E-16, -1.610000000000000098 ) ) ;
#890 = EDGE_LOOP ( 'NONE', ( #3130, #1702, #3800, #649 ) ) ;
#891 = CARTESIAN_POINT ( 'NONE',  ( 0.000000000000000000, 0.000000000000000000, -30.00000000000000000 ) ) ;
#892 = EDGE_CURVE ( 'NONE', #102, #3822, #428, .T. ) ;
#893 = MECHANICAL_DESIGN_GEOMETRIC_PRESENTATION_REPRESENTATION (  '', ( #2124 ), #198 ) ;
#894 = AXIS2_PLACEMENT_3D ( 'NONE', #2296, #1423, #1955 ) ;
#895 = AXIS2_PLACEMENT_3D ( 'NONE', #1164, #859, #1728 ) ;
#896 = ORIENTED_EDGE ( 'NONE', *, *, #134, .T. ) ;
#897 = CARTESIAN_POINT ( 'NONE',  ( -82.00000000000000000, 0.000000000000000000, 3.000000000000000000 ) ) ;
#898 =( NAMED_UNIT ( * ) SI_UNIT ( $, .STERADIAN. ) SOLID_ANGLE_UNIT ( ) );
#899 = PRODUCT_DEFINITION ( 'UNKNOWN', '', #1103, #165 ) ;
#900 = VECTOR ( 'NONE', #3282, 1000.000000000000000 ) ;
#901 = ORIENTED_EDGE ( 'NONE', *, *, #191, .F. ) ;
#902 = DIRECTION ( 'NONE',  ( -0.000000000000000000, -0.000000000000000000, -1.000000000000000000 ) ) ;
#903 = AXIS2_PLACEMENT_3D ( 'NONE', #3436, #1670, #2854 ) ;
#904 = DIRECTION ( 'NONE',  ( 0.000000000000000000, 0.000000000000000000, 1.000000000000000000 ) ) ;
#905 = EDGE_CURVE ( 'NONE', #1737, #2422, #2837, .T. ) ;
#906 = AXIS2_PLACEMENT_3D ( 'NONE', #837, #3174, #2024 ) ;
#907 = ORIENTED_EDGE ( 'NONE', *, *, #566, .F. ) ;
#908 =( GEOMETRIC_REPRESENTATION_CONTEXT ( 3 ) GLOBAL_UNCERTAINTY_ASSIGNED_CONTEXT ( ( #3619 ) ) GLOBAL_UNIT_ASSIGNED_CONTEXT ( ( #884, #1793, #924 ) ) REPRESENTATION_CONTEXT ( 'NONE', 'WORKASPACE' ) );
#909 = AXIS2_PLACEMENT_3D ( 'NONE', #692, #2213, #1874 ) ;
#910 = VERTEX_POINT ( 'NONE', #1069 ) ;
#911 = EDGE_LOOP ( 'NONE', ( #1275, #2494 ) ) ;
#912 = AXIS2_PLACEMENT_3D ( 'NONE', #2414, #2706, #1228 ) ;
#913 = AXIS2_PLACEMENT_3D ( 'NONE', #1710, #2640, #3753 ) ;
#914 = LINE ( 'NONE', #2097, #900 ) ;
#915 = CIRCLE ( 'NONE', #2590, 5.000000000000004441 ) ;
#916 = VERTEX_POINT ( 'NONE', #371 ) ;
#917 = CARTESIAN_POINT ( 'NONE',  ( 1.300000000000000044, -1.443375672974064328, 2.168404344971008868E-16 ) ) ;
#918 = CARTESIAN_POINT ( 'NONE',  ( 20.00000000000000000, 0.000000000000000000, -20.00000000000000000 ) ) ;
#919 = FILL_AREA_STYLE ('',( #359 ) ) ;
#920 = DIRECTION ( 'NONE',  ( 0.000000000000000000, 0.000000000000000000, 1.000000000000000000 ) ) ;
#921 = ORIENTED_EDGE ( 'NONE', *, *, #437, .T. ) ;
#922 = CARTESIAN_POINT ( 'NONE',  ( 1.820000000000000062, 0.000000000000000000, 0.000000000000000000 ) ) ;
#923 = CARTESIAN_POINT ( 'NONE',  ( 25.15000000000000213, 3.079986699855593473E-15, 0.000000000000000000 ) ) ;
#924 =( NAMED_UNIT ( * ) SI_UNIT ( $, .STERADIAN. ) SOLID_ANGLE_UNIT ( ) );
#925 = DIRECTION ( 'NONE',  ( 0.000000000000000000, 0.000000000000000000, 1.000000000000000000 ) ) ;
#926 = VERTEX_POINT ( 'NONE', #754 ) ;
#927 = ORIENTED_EDGE ( 'NONE', *, *, #3644, .T. ) ;
#928 = CARTESIAN_POINT ( 'NONE',  ( -1.649999999999998579, 0.000000000000000000, -14.99999999999999645 ) ) ;
#929 = VERTEX_POINT ( 'NONE', #1646 ) ;
#930 = EDGE_CURVE ( 'NONE', #1166, #1798, #1457, .T. ) ;
#931 = CARTESIAN_POINT ( 'NONE',  ( 8.673617379884035472E-16, 0.000000000000000000, 0.000000000000000000 ) ) ;
#932 = EDGE_LOOP ( 'NONE', ( #2133, #2546, #3592, #3528, #1761, #330 ) ) ;
#933 = DIRECTION ( 'NONE',  ( 1.000000000000000000, 0.000000000000000000, 0.000000000000000000 ) ) ;
#934 = CARTESIAN_POINT ( 'NONE',  ( 1.300000000000000044, 0.7216878364870328300, -1.250000000000000000 ) ) ;
#935 = DIRECTION ( 'NONE',  ( -1.000000000000000000, 5.843967824224479992E-17, -1.241531209392319534E-18 ) ) ;
#936 = DIRECTION ( 'NONE',  ( -1.000000000000000000, 0.000000000000000000, 0.000000000000000000 ) ) ;
#937 = ADVANCED_FACE ( 'NONE', ( #3402, #454 ), #2465, .T. ) ;
#938 = DIRECTION ( 'NONE',  ( 1.000000000000000000, 0.000000000000000000, 0.000000000000000000 ) ) ;
#939 = PRESENTATION_STYLE_ASSIGNMENT (( #2140 ) ) ;
#940 = CARTESIAN_POINT ( 'NONE',  ( 1.600000000000000089, 0.000000000000000000, 0.000000000000000000 ) ) ;
#941 = CARTESIAN_POINT ( 'NONE',  ( -82.50000000000000000, -19.84313483298442904, -30.00000000000000000 ) ) ;
#942 = ORIENTED_EDGE ( 'NONE', *, *, #3532, .T. ) ;
#943 = EDGE_CURVE ( 'NONE', #1799, #2993, #2254, .T. ) ;
#944 = ORIENTED_EDGE ( 'NONE', *, *, #1158, .F. ) ;
#945 = LINE ( 'NONE', #2951, #1884 ) ;
#946 = ORIENTED_EDGE ( 'NONE', *, *, #1525, .F. ) ;
#947 = CARTESIAN_POINT ( 'NONE',  ( 0.000000000000000000, 0.000000000000000000, 1.622657008870242981E-16 ) ) ;
#948 = TOROIDAL_SURFACE ( 'NONE', #2565, 23.82500000000000284, 1.324999999999999956 ) ;
#949 = EDGE_LOOP ( 'NONE', ( #1236, #873, #1842, #2456 ) ) ;
#950 = DIRECTION ( 'NONE',  ( -0.5000000000000042188, 1.060575238724903710E-16, -0.8660254037844361541 ) ) ;
#951 = DIRECTION ( 'NONE',  ( 0.000000000000000000, 0.000000000000000000, 1.000000000000000000 ) ) ;
#952 = AXIS2_PLACEMENT_3D ( 'NONE', #2980, #2082, #70 ) ;
#953 =( LENGTH_UNIT ( ) NAMED_UNIT ( * ) SI_UNIT ( .MILLI., .METRE. ) );
#954 = AXIS2_PLACEMENT_3D ( 'NONE', #14, #1256, #3035 ) ;
#955 = ADVANCED_FACE ( 'NONE', ( #3098 ), #3714, .T. ) ;
#956 = CARTESIAN_POINT ( 'NONE',  ( 0.000000000000000000, 0.7216878364870329410, 1.249999999999999778 ) ) ;
#957 = DIRECTION ( 'NONE',  ( -0.000000000000000000, -0.000000000000000000, -1.000000000000000000 ) ) ;
#958 = APPLICATION_CONTEXT ( 'automotive_design' ) ;
#959 = AXIS2_PLACEMENT_3D ( 'NONE', #3710, #1932, #367 ) ;
#960=STYLED_ITEM('',(#3881),#3213);
#961 = SHAPE_REPRESENTATION ( 'specimen holder', ( #2207 ), #908 ) ;
#962 = DIRECTION ( 'NONE',  ( 0.000000000000000000, 0.000000000000000000, 1.000000000000000000 ) ) ;
#963 = DIRECTION ( 'NONE',  ( -1.000000000000000000, 0.000000000000000000, 0.000000000000000000 ) ) ;
#964 = VERTEX_POINT ( 'NONE', #1919 ) ;
#965 = FACE_BOUND ( 'NONE', #415, .T. ) ;
#966 = ORIENTED_EDGE ( 'NONE', *, *, #3281, .F. ) ;
#967 = LINE ( 'NONE', #1786, #578 ) ;
#968 =( GEOMETRIC_REPRESENTATION_CONTEXT ( 3 ) GLOBAL_UNCERTAINTY_ASSIGNED_CONTEXT ( ( #3201 ) ) GLOBAL_UNIT_ASSIGNED_CONTEXT ( ( #2883, #3143, #1928 ) ) REPRESENTATION_CONTEXT ( 'NONE', 'WORKASPACE' ) );
#969 = VECTOR ( 'NONE', #1622, 1000.000000000000000 ) ;
#970 = EDGE_CURVE ( 'NONE', #2875, #2365, #2767, .T. ) ;
#971 = VECTOR ( 'NONE', #1427, 1000.000000000000114 ) ;
#972 = DIRECTION ( 'NONE',  ( -1.000000000000000000, 0.000000000000000000, 0.000000000000000000 ) ) ;
#973 = VERTEX_POINT ( 'NONE', #3419 ) ;
#974 = CARTESIAN_POINT ( 'NONE',  ( -3.749999999999998224, -29.76470224947664533, -30.00000000000000000 ) ) ;
#975 = CARTESIAN_POINT ( 'NONE',  ( -70.00000000000000000, -21.41798680385620202, -30.00000000000000000 ) ) ;
#976 = TOROIDAL_SURFACE ( 'NONE', #2291, 23.82500000000000284, 1.324999999999999956 ) ;
#977 = EDGE_CURVE ( 'NONE', #3418, #3091, #593, .T. ) ;
#978 = CARTESIAN_POINT ( 'NONE',  ( 0.000000000000000000, 0.000000000000000000, -20.00000000000000000 ) ) ;
#979 = CARTESIAN_POINT ( 'NONE',  ( 1.999999999999999112, 2.449293598294705428E-16, -20.00000000000000000 ) ) ;
#980 = FILL_AREA_STYLE_COLOUR ( '', #40 ) ;
#981 = ADVANCED_FACE ( 'NONE', ( #3358 ), #2481, .T. ) ;
#982 = DIRECTION ( 'NONE',  ( 0.000000000000000000, 1.000000000000000000, 1.224646799147353207E-16 ) ) ;
#983 = LINE ( 'NONE', #129, #513 ) ;
#984 = EDGE_LOOP ( 'NONE', ( #539, #3539, #2270, #1291, #3298 ) ) ;
#985 = PRESENTATION_STYLE_ASSIGNMENT (( #81 ) ) ;
#986 = EDGE_LOOP ( 'NONE', ( #433, #3523, #558, #473 ) ) ;
#987 = CARTESIAN_POINT ( 'NONE',  ( -3.750000000000001776, -29.76470224947664178, 0.000000000000000000 ) ) ;
#988 = B_SPLINE_CURVE_WITH_KNOTS ( 'NONE', 3,
 ( #1809, #2416, #642, #92 ),
 .UNSPECIFIED., .F., .F.,
 ( 4, 4 ),
 ( 0.000000000000000000, 1.000000000000000000 ),
 .UNSPECIFIED. ) ;
#989 = CARTESIAN_POINT ( 'NONE',  ( 2.400000000000000799, 2.449293598294705428E-16, -1.999999999999999112 ) ) ;
#990 = ORIENTED_EDGE ( 'NONE', *, *, #1849, .T. ) ;
#991 = DIRECTION ( 'NONE',  ( -0.000000000000000000, -0.000000000000000000, -1.000000000000000000 ) ) ;
#992 = DIRECTION ( 'NONE',  ( -0.000000000000000000, -0.000000000000000000, -1.000000000000000000 ) ) ;
#993 = CARTESIAN_POINT ( 'NONE',  ( 0.000000000000000000, 0.000000000000000000, 0.000000000000000000 ) ) ;
#994 = PRODUCT_DEFINITION_SHAPE ( 'NONE', 'NONE',  #2395 ) ;
#995 = CARTESIAN_POINT ( 'NONE',  ( 1.300000000000000044, 0.000000000000000000, 0.000000000000000000 ) ) ;
#996 = DIRECTION ( 'NONE',  ( -0.000000000000000000, 0.000000000000000000, 1.000000000000000000 ) ) ;
#997 = SURFACE_SIDE_STYLE ('',( #2471 ) ) ;
#998 = CARTESIAN_POINT ( 'NONE',  ( -3.799999999999999378, 0.000000000000000000, 0.000000000000000000 ) ) ;
#999 = DIRECTION ( 'NONE',  ( -0.000000000000000000, -0.000000000000000000, -1.000000000000000000 ) ) ;
#1000 = EDGE_CURVE ( 'NONE', #1302, #2909, #1402, .T. ) ;
#1001 = ORIENTED_EDGE ( 'NONE', *, *, #347, .T. ) ;
#1002 = PRESENTATION_STYLE_ASSIGNMENT (( #3646 ) ) ;
#1003 = VERTEX_POINT ( 'NONE', #3667 ) ;
#1004 = DIRECTION ( 'NONE',  ( -0.000000000000000000, -0.000000000000000000, -1.000000000000000000 ) ) ;
#1005 = PRODUCT_DEFINITION_SHAPE ( 'NONE', 'NONE',  #537 ) ;
#1006 = FACE_OUTER_BOUND ( 'NONE', #3126, .T. ) ;
#1007 = ORIENTED_EDGE ( 'NONE', *, *, #3276, .F. ) ;
#1008 = CARTESIAN_POINT ( 'NONE',  ( -3.750000000000001776, -29.76470224947664178, -4.999999999999997335 ) ) ;
#1009 = EDGE_CURVE ( 'NONE', #1780, #573, #3113, .T. ) ;
#1010 = FACE_OUTER_BOUND ( 'NONE', #3073, .T. ) ;
#1011 = CARTESIAN_POINT ( 'NONE',  ( 0.000000000000000000, 0.7216878364870328300, 1.249999999999999778 ) ) ;
#1012 = AXIS2_PLACEMENT_3D ( 'NONE', #360, #2430, #2449 ) ;
#1013 = CYLINDRICAL_SURFACE ( 'NONE', #1035, 34.99999999999999289 ) ;
#1014 = ORIENTED_EDGE ( 'NONE', *, *, #665, .F. ) ;
#1015 = CARTESIAN_POINT ( 'NONE',  ( 0.000000000000000000, 0.000000000000000000, 4.999999999999997335 ) ) ;
#1016 = PRODUCT_RELATED_PRODUCT_CATEGORY ( 'part', '', ( #3397 ) ) ;
#1017 =( GEOMETRIC_REPRESENTATION_CONTEXT ( 3 ) GLOBAL_UNCERTAINTY_ASSIGNED_CONTEXT ( ( #1372 ) ) GLOBAL_UNIT_ASSIGNED_CONTEXT ( ( #747, #1597, #114 ) ) REPRESENTATION_CONTEXT ( 'NONE', 'WORKASPACE' ) );
#1018 = AXIS2_PLACEMENT_3D ( 'NONE', #1015, #3387, #2507 ) ;
#1019 = VECTOR ( 'NONE', #2726, 1000.000000000000114 ) ;
#1020 = DIRECTION ( 'NONE',  ( 0.000000000000000000, 0.000000000000000000, 1.000000000000000000 ) ) ;
#1021 = DIRECTION ( 'NONE',  ( 0.3871933609746164295, 0.9219985364506716463, -2.410490433790583766E-18 ) ) ;
#1022 = EDGE_CURVE ( 'NONE', #2012, #2149, #2017, .T. ) ;
#1023 = AXIS2_PLACEMENT_3D ( 'NONE', #917, #284, #2703 ) ;
#1024 = EDGE_LOOP ( 'NONE', ( #862, #732, #2751, #550 ) ) ;
#1025 = FILL_AREA_STYLE ('',( #2735 ) ) ;
#1026 = ORIENTED_EDGE ( 'NONE', *, *, #2239, .F. ) ;
#1027 = AXIS2_PLACEMENT_3D ( 'NONE', #2233, #2526, #2775 ) ;
#1028 = CARTESIAN_POINT ( 'NONE',  ( -80.00000000000000000, 0.000000000000000000, -5.000000000000000000 ) ) ;
#1029 = DIRECTION ( 'NONE',  ( -1.000000000000000000, -0.000000000000000000, -0.000000000000000000 ) ) ;
#1030 = ORIENTED_EDGE ( 'NONE', *, *, #3165, .T. ) ;
#1031 = DIRECTION ( 'NONE',  ( -1.000000000000000000, 0.000000000000000000, 0.000000000000000000 ) ) ;
#1032 = AXIS2_PLACEMENT_3D ( 'NONE', #1070, #2548, #3734 ) ;
#1033 = DIRECTION ( 'NONE',  ( -0.000000000000000000, -0.000000000000000000, -1.000000000000000000 ) ) ;
#1034 = CARTESIAN_POINT ( 'NONE',  ( 1.300000000000000044, 0.000000000000000000, 0.000000000000000000 ) ) ;
#1035 = AXIS2_PLACEMENT_3D ( 'NONE', #2174, #3363, #722 ) ;
#1036 =( NAMED_UNIT ( * ) SI_UNIT ( $, .STERADIAN. ) SOLID_ANGLE_UNIT ( ) );
#1037 = DIRECTION ( 'NONE',  ( 1.000000000000000000, 0.000000000000000000, 0.000000000000000000 ) ) ;
#1038 = CARTESIAN_POINT ( 'NONE',  ( -3.750000000000004441, 29.76470224947664533, 5.000000000000000000 ) ) ;
#1039 = FILL_AREA_STYLE_COLOUR ( '', #153 ) ;
#1040 =( GEOMETRIC_REPRESENTATION_CONTEXT ( 3 ) GLOBAL_UNCERTAINTY_ASSIGNED_CONTEXT ( ( #1958 ) ) GLOBAL_UNIT_ASSIGNED_CONTEXT ( ( #3266, #244, #865 ) ) REPRESENTATION_CONTEXT ( 'NONE', 'WORKASPACE' ) );
#1041 = VECTOR ( 'NONE', #3490, 1000.000000000000000 ) ;
#1042 = ADVANCED_FACE ( 'NONE', ( #2538 ), #3161, .F. ) ;
#1043 = ITEM_DEFINED_TRANSFORMATION ( 'NONE', 'NONE', #402,  #2207 ) ;
#1044 = CARTESIAN_POINT ( 'NONE',  ( 1.300000000000000044, -1.443375672974063884, -3.691112476943992763E-18 ) ) ;
#1045 = CARTESIAN_POINT ( 'NONE',  ( 23.82500000000000284, 2.917720998968569322E-15, 0.000000000000000000 ) ) ;
#1046 = PRODUCT ( 'o-rings series a_iso_O-ring 45x2.65-A-ISO 3601-1', 'o-rings series a_iso_O-ring 45x2.65-A-ISO 3601-1', '', ( #3427 ) ) ;
#1047 = EDGE_CURVE ( 'NONE', #3785, #1824, #3150, .T. ) ;
#1048 = ORIENTED_EDGE ( 'NONE', *, *, #1638, .T. ) ;
#1049 = ORIENTED_EDGE ( 'NONE', *, *, #3120, .F. ) ;
#1050 = FACE_OUTER_BOUND ( 'NONE', #2059, .T. ) ;
#1051 = EDGE_CURVE ( 'NONE', #1495, #691, #2285, .T. ) ;
#1052 = EDGE_CURVE ( 'NONE', #868, #3489, #184, .T. ) ;
#1053 = CARTESIAN_POINT ( 'NONE',  ( 1.600000000000000089, 0.000000000000000000, 0.000000000000000000 ) ) ;
#1054 = ORIENTED_EDGE ( 'NONE', *, *, #275, .T. ) ;
#1055 = CARTESIAN_POINT ( 'NONE',  ( 2.199999999999999734, 0.000000000000000000, 0.000000000000000000 ) ) ;
#1056 = DIRECTION ( 'NONE',  ( -1.000000000000000000, 0.000000000000000000, 0.000000000000000000 ) ) ;
#1057 = LINE ( 'NONE', #395, #3563 ) ;
#1058 = DIRECTION ( 'NONE',  ( 0.000000000000000000, 0.000000000000000000, 1.000000000000000000 ) ) ;
#1059 = DIRECTION ( 'NONE',  ( -0.000000000000000000, -0.000000000000000000, -1.000000000000000000 ) ) ;
#1060 = FACE_OUTER_BOUND ( 'NONE', #3394, .T. ) ;
#1061 = PRODUCT_CONTEXT ( 'NONE', #3170, 'mechanical' ) ;
#1062 = DIRECTION ( 'NONE',  ( -0.000000000000000000, 0.000000000000000000, -1.000000000000000000 ) ) ;
#1063 = ORIENTED_EDGE ( 'NONE', *, *, #164, .T. ) ;
#1064 = ORIENTED_EDGE ( 'NONE', *, *, #2379, .F. ) ;
#1065 = DIRECTION ( 'NONE',  ( 0.000000000000000000, 0.000000000000000000, 1.000000000000000000 ) ) ;
#1066 = EDGE_CURVE ( 'NONE', #2840, #2084, #3460, .T. ) ;
#1067 = CARTESIAN_POINT ( 'NONE',  ( 0.000000000000000000, 0.000000000000000000, -14.99999999999999645 ) ) ;
#1068 = VERTEX_POINT ( 'NONE', #2932 ) ;
#1069 = CARTESIAN_POINT ( 'NONE',  ( -3.749999999999998224, 29.76470224947664533, 0.000000000000000000 ) ) ;
#1070 = CARTESIAN_POINT ( 'NONE',  ( 0.000000000000000000, 0.000000000000000000, 0.000000000000000000 ) ) ;
#1071 = CARTESIAN_POINT ( 'NONE',  ( 30.00000000000000000, 0.000000000000000000, -30.00000000000000000 ) ) ;
#1072 = PRODUCT_DEFINITION_SHAPE ( 'NONE', 'NONE',  #3839 ) ;
#1073 = ORIENTED_EDGE ( 'NONE', *, *, #1212, .T. ) ;
#1074 = DIRECTION ( 'NONE',  ( 0.000000000000000000, 0.000000000000000000, -1.000000000000000000 ) ) ;
#1075 = DIRECTION ( 'NONE',  ( 0.000000000000000000, 0.000000000000000000, 1.000000000000000000 ) ) ;
#1076 = EDGE_CURVE ( 'NONE', #868, #821, #3171, .T. ) ;
#1077 = AXIS2_PLACEMENT_3D ( 'NONE', #128, #1951, #1325 ) ;
#1078 = CONTEXT_DEPENDENT_SHAPE_REPRESENTATION ( #2972, #625 ) ;
#1079 = DIRECTION ( 'NONE',  ( 1.000000000000000000, 0.000000000000000000, 0.000000000000000000 ) ) ;
#1080 = AXIS2_PLACEMENT_3D ( 'NONE', #3179, #530, #2863 ) ;
#1081 = AXIS2_PLACEMENT_3D ( 'NONE', #993, #3115, #2549 ) ;
#1082 = ORIENTED_EDGE ( 'NONE', *, *, #2401, .F. ) ;
#1083 = DIRECTION ( 'NONE',  ( 0.1250000000000000833, 0.9921567416492215186, -0.000000000000000000 ) ) ;
#1084 = ORIENTED_EDGE ( 'NONE', *, *, #2901, .T. ) ;
#1085 = CARTESIAN_POINT ( 'NONE',  ( 1.300000000000000044, -0.7216878364870318308, 1.249999999999999778 ) ) ;
#1086 = AXIS2_PLACEMENT_3D ( 'NONE', #2752, #84, #689 ) ;
#1087 = CIRCLE ( 'NONE', #2509, 0.8999999999999999112 ) ;
#1088 = CARTESIAN_POINT ( 'NONE',  ( 2.400000000000000799, 0.000000000000000000, 2.199999999999999289 ) ) ;
#1089 = EDGE_LOOP ( 'NONE', ( #2639, #1113, #2464, #921 ) ) ;
#1090 = FACE_OUTER_BOUND ( 'NONE', #2921, .T. ) ;
#1091 = CARTESIAN_POINT ( 'NONE',  ( 0.000000000000000000, 0.000000000000000000, -15.70000000000000284 ) ) ;
#1092 = EDGE_CURVE ( 'NONE', #2875, #3067, #2650, .T. ) ;
#1093 = CIRCLE ( 'NONE', #221, 1.249999999999999778 ) ;
#1094 = EDGE_LOOP ( 'NONE', ( #1195, #2367 ) ) ;
#1095 = CARTESIAN_POINT ( 'NONE',  ( -23.82500000000000284, 0.000000000000000000, 0.000000000000000000 ) ) ;
#1096 = CARTESIAN_POINT ( 'NONE',  ( 1.820000000000000062, 3.799999999999999378, 0.000000000000000000 ) ) ;
#1097 = CIRCLE ( 'NONE', #3701, 3.799999999999999378 ) ;
#1098 = MECHANICAL_DESIGN_GEOMETRIC_PRESENTATION_REPRESENTATION (  '', ( #3026 ), #1155 ) ;
#1099 = EDGE_CURVE ( 'NONE', #2038, #2858, #512, .T. ) ;
#1100 = EDGE_CURVE ( 'NONE', #1755, #2149, #3706, .T. ) ;
#1101 = CIRCLE ( 'NONE', #1965, 2.000000000000001776 ) ;
#1102 = CARTESIAN_POINT ( 'NONE',  ( 0.000000000000000000, 0.000000000000000000, 0.000000000000000000 ) ) ;
#1103 = PRODUCT_DEFINITION_FORMATION_WITH_SPECIFIED_SOURCE ( 'ANY', '', #3567, .NOT_KNOWN. ) ;
#1104 = VECTOR ( 'NONE', #1788, 1000.000000000000000 ) ;
#1105 = VERTEX_POINT ( 'NONE', #2333 ) ;
#1106 = FACE_OUTER_BOUND ( 'NONE', #230, .T. ) ;
#1107 = VERTEX_POINT ( 'NONE', #1999 ) ;
#1108 = DIRECTION ( 'NONE',  ( 1.000000000000000000, 0.000000000000000000, 0.000000000000000000 ) ) ;
#1109 = ORIENTED_EDGE ( 'NONE', *, *, #1617, .T. ) ;
#1110 = DIRECTION ( 'NONE',  ( 0.000000000000000000, 0.000000000000000000, -1.000000000000000000 ) ) ;
#1111 = CARTESIAN_POINT ( 'NONE',  ( 2.000000000000001776, 0.000000000000000000, -24.00000000000000000 ) ) ;
#1112 = PRODUCT_RELATED_PRODUCT_CATEGORY ( 'part', '', ( #1906 ) ) ;
#1113 = ORIENTED_EDGE ( 'NONE', *, *, #2629, .F. ) ;
#1114 = DIRECTION ( 'NONE',  ( 0.000000000000000000, 0.000000000000000000, 1.000000000000000000 ) ) ;
#1115 = SURFACE_STYLE_USAGE ( .BOTH. , #3781 ) ;
#1116 = CARTESIAN_POINT ( 'NONE',  ( -78.00000000000000000, 2.449293598294708880E-16, -5.000000000000000000 ) ) ;
#1117 = FACE_OUTER_BOUND ( 'NONE', #1586, .T. ) ;
#1118 = EDGE_LOOP ( 'NONE', ( #1839, #264, #1666, #669 ) ) ;
#1119 = DIRECTION ( 'NONE',  ( 0.9921567416492215186, 0.1250000000000001665, 0.000000000000000000 ) ) ;
#1120 = EDGE_LOOP ( 'NONE', ( #2830, #326, #2091, #1837 ) ) ;
#1121 = EDGE_CURVE ( 'NONE', #1151, #3615, #1672, .T. ) ;
#1122 = FACE_OUTER_BOUND ( 'NONE', #21, .T. ) ;
#1123 = ORIENTED_EDGE ( 'NONE', *, *, #2637, .T. ) ;
#1124 = CARTESIAN_POINT ( 'NONE',  ( -82.50000000000000000, 19.84313483298442193, -30.00000000000000000 ) ) ;
#1125 = DIRECTION ( 'NONE',  ( -1.000000000000000000, 0.000000000000000000, 0.000000000000000000 ) ) ;
#1126 = EDGE_CURVE ( 'NONE', #355, #2934, #3519, .T. ) ;
#1127 = ORIENTED_EDGE ( 'NONE', *, *, #1126, .F. ) ;
#1128 = CARTESIAN_POINT ( 'NONE',  ( -80.00000000000000000, 0.000000000000000000, -5.000000000000000000 ) ) ;
#1129 = CARTESIAN_POINT ( 'NONE',  ( -83.12500000000000000, -24.80391854123052653, 5.000000000000000000 ) ) ;
#1130 = ORIENTED_EDGE ( 'NONE', *, *, #461, .T. ) ;
#1131 = FACE_OUTER_BOUND ( 'NONE', #65, .T. ) ;
#1132 = SURFACE_STYLE_USAGE ( .BOTH. , #322 ) ;
#1133 = EDGE_CURVE ( 'NONE', #1954, #494, #858, .T. ) ;
#1134 = TOROIDAL_SURFACE ( 'NONE', #1501, 2.199999999999999289, 0.2000000000000000111 ) ;
#1135 = CARTESIAN_POINT ( 'NONE',  ( -87.59475001958765006, -18.54744454438354495, 3.811325414771110864 ) ) ;
#1136 = VERTEX_POINT ( 'NONE', #1376 ) ;
#1137 = EDGE_CURVE ( 'NONE', #143, #1068, #1101, .T. ) ;
#1138 = COLOUR_RGB ( '',1.000000000000000000, 0.9490196078431372140, 0.9098039215686274384 ) ;
#1139 = CIRCLE ( 'NONE', #3191, 1.250000000000000222 ) ;
#1140 = ADVANCED_FACE ( 'NONE', ( #1090 ), #813, .F. ) ;
#1141 = FACE_OUTER_BOUND ( 'NONE', #1390, .T. ) ;
#1142 = ORIENTED_EDGE ( 'NONE', *, *, #1099, .F. ) ;
#1143 = CARTESIAN_POINT ( 'NONE',  ( 1.300000000000000044, 1.443375672974065216, 7.017607234860990640E-28 ) ) ;
#1144 = ADVANCED_FACE ( 'NONE', ( #3825 ), #2279, .T. ) ;
#1145 = AXIS2_PLACEMENT_3D ( 'NONE', #95, #2202, #2745 ) ;
#1146 = CARTESIAN_POINT ( 'NONE',  ( 1.300000000000000044, 0.000000000000000000, 0.000000000000000000 ) ) ;
#1147 = AXIS2_PLACEMENT_3D ( 'NONE', #3323, #3017, #3299 ) ;
#1148 = VERTEX_POINT ( 'NONE', #1413 ) ;
#1149 = CARTESIAN_POINT ( 'NONE',  ( 1.300000000000000044, 0.000000000000000000, 0.000000000000000000 ) ) ;
#1150 = SURFACE_STYLE_FILL_AREA ( #3582 ) ;
#1151 = VERTEX_POINT ( 'NONE', #3205 ) ;
#1152 = CYLINDRICAL_SURFACE ( 'NONE', #1814, 1.999999999999999112 ) ;
#1153 = TOROIDAL_SURFACE ( 'NONE', #2523, 2.899999999999999911, 0.8999999999999999112 ) ;
#1154 =( GEOMETRIC_REPRESENTATION_CONTEXT ( 3 ) GLOBAL_UNCERTAINTY_ASSIGNED_CONTEXT ( ( #1916 ) ) GLOBAL_UNIT_ASSIGNED_CONTEXT ( ( #2623, #1473, #3811 ) ) REPRESENTATION_CONTEXT ( 'NONE', 'WORKASPACE' ) );
#1155 =( GEOMETRIC_REPRESENTATION_CONTEXT ( 3 ) GLOBAL_UNCERTAINTY_ASSIGNED_CONTEXT ( ( #1207 ) ) GLOBAL_UNIT_ASSIGNED_CONTEXT ( ( #741, #1628, #1036 ) ) REPRESENTATION_CONTEXT ( 'NONE', 'WORKASPACE' ) );
#1156 = DIRECTION ( 'NONE',  ( -1.000000000000000000, -0.000000000000000000, -0.000000000000000000 ) ) ;
#1157 = ORIENTED_EDGE ( 'NONE', *, *, #34, .T. ) ;
#1158 = EDGE_CURVE ( 'NONE', #283, #673, #2601, .T. ) ;
#1159 = VECTOR ( 'NONE', #553, 1000.000000000000000 ) ;
#1160 = ORIENTED_EDGE ( 'NONE', *, *, #3532, .F. ) ;
#1161 = SURFACE_SIDE_STYLE ('',( #1520 ) ) ;
#1162 = EDGE_LOOP ( 'NONE', ( #2023, #793, #1218, #1178 ) ) ;
#1163 = DIRECTION ( 'NONE',  ( -0.000000000000000000, 0.5000000000000001110, 0.8660254037844385966 ) ) ;
#1164 = CARTESIAN_POINT ( 'NONE',  ( 1.300000000000000044, -0.7216878364870317197, 1.250000000000000000 ) ) ;
#1165 = PRODUCT_CONTEXT ( 'NONE', #3024, 'mechanical' ) ;
#1166 = VERTEX_POINT ( 'NONE', #202 ) ;
#1167 = DIRECTION ( 'NONE',  ( -0.000000000000000000, -0.000000000000000000, -1.000000000000000000 ) ) ;
#1168 = CARTESIAN_POINT ( 'NONE',  ( 8.673617379884035472E-16, -1.899999999999999689, -3.490243377569955568E-16 ) ) ;
#1169 = ORIENTED_EDGE ( 'NONE', *, *, #707, .T. ) ;
#1170 = FACE_OUTER_BOUND ( 'NONE', #2696, .T. ) ;
#1171 = DIRECTION ( 'NONE',  ( -0.000000000000000000, 0.000000000000000000, -1.000000000000000000 ) ) ;
#1172 = EDGE_CURVE ( 'NONE', #3629, #2659, #1396, .T. ) ;
#1173 = FACE_OUTER_BOUND ( 'NONE', #364, .T. ) ;
#1174 = ORIENTED_EDGE ( 'NONE', *, *, #3728, .F. ) ;
#1175 = APPLICATION_CONTEXT ( 'automotive_design' ) ;
#1176 = ORIENTED_EDGE ( 'NONE', *, *, #437, .F. ) ;
#1177 = CARTESIAN_POINT ( 'NONE',  ( 2.200000000000000622, 2.694222958124176020E-16, -2.199999999999999289 ) ) ;
#1178 = ORIENTED_EDGE ( 'NONE', *, *, #3801, .T. ) ;
#1179 = CARTESIAN_POINT ( 'NONE',  ( -3.749999999999998224, 29.76470224947664533, 0.000000000000000000 ) ) ;
#1180 = ADVANCED_FACE ( 'NONE', ( #831 ), #2473, .F. ) ;
#1181 = DIRECTION ( 'NONE',  ( -0.000000000000000000, -0.000000000000000000, -1.000000000000000000 ) ) ;
#1182 = EDGE_LOOP ( 'NONE', ( #3240, #3707, #2855, #1049 ) ) ;
#1183 = CARTESIAN_POINT ( 'NONE',  ( 0.000000000000000000, 0.000000000000000000, 0.000000000000000000 ) ) ;
#1184 = LINE ( 'NONE', #38, #2889 ) ;
#1185 = CARTESIAN_POINT ( 'NONE',  ( -80.00000000000000000, 0.000000000000000000, -4.999999999999997335 ) ) ;
#1186 = ADVANCED_FACE ( 'NONE', ( #76 ), #43, .T. ) ;
#1187 = VERTEX_POINT ( 'NONE', #666 ) ;
#1188 = DIRECTION ( 'NONE',  ( -1.000000000000000000, -0.000000000000000000, -0.000000000000000000 ) ) ;
#1189 = CARTESIAN_POINT ( 'NONE',  ( 1.300000000000000044, -0.7216878364870318308, -1.250000000000000000 ) ) ;
#1190 = CARTESIAN_POINT ( 'NONE',  ( 1.820000000000000062, 0.000000000000000000, 0.000000000000000000 ) ) ;
#1191 = ORIENTED_EDGE ( 'NONE', *, *, #3705, .T. ) ;
#1192 = TOROIDAL_SURFACE ( 'NONE', #1316, 23.82500000000000284, 1.324999999999999956 ) ;
#1193 = ORIENTED_EDGE ( 'NONE', *, *, #1172, .T. ) ;
#1194 = DIRECTION ( 'NONE',  ( -0.000000000000000000, -0.000000000000000000, 1.000000000000000000 ) ) ;
#1195 = ORIENTED_EDGE ( 'NONE', *, *, #1897, .F. ) ;
#1196 = CARTESIAN_POINT ( 'NONE',  ( 0.000000000000000000, 0.000000000000000000, 0.000000000000000000 ) ) ;
#1197 = AXIS2_PLACEMENT_3D ( 'NONE', #352, #1219, #2421 ) ;
#1198 = CIRCLE ( 'NONE', #3185, 7.000000000000000000 ) ;
#1199 = AXIS2_PLACEMENT_3D ( 'NONE', #1111, #2352, #2642 ) ;
#1200 = EDGE_LOOP ( 'NONE', ( #1307, #497, #50, #2776, #2114 ) ) ;
#1201 = DIRECTION ( 'NONE',  ( -1.000000000000000000, -0.000000000000000000, -0.000000000000000000 ) ) ;
#1202 = CARTESIAN_POINT ( 'NONE',  ( -90.00000000000000000, -17.32050807568877815, -30.00000000000000000 ) ) ;
#1203 = PRESENTATION_STYLE_ASSIGNMENT (( #1565 ) ) ;
#1204 = CARTESIAN_POINT ( 'NONE',  ( 0.000000000000000000, 0.000000000000000000, 0.000000000000000000 ) ) ;
#1205 = EDGE_CURVE ( 'NONE', #2381, #1598, #3826, .T. ) ;
#1206 = PRODUCT_DEFINITION_SHAPE ( 'NONE', 'NONE',  #3366 ) ;
#1207 = UNCERTAINTY_MEASURE_WITH_UNIT (LENGTH_MEASURE( 1.000000000000000082E-05 ), #741, 'distance_accuracy_value', 'NONE');
#1208 = ORIENTED_EDGE ( 'NONE', *, *, #3166, .F. ) ;
#1209 = FACE_OUTER_BOUND ( 'NONE', #984, .T. ) ;
#1210 = VECTOR ( 'NONE', #3294, 1000.000000000000000 ) ;
#1211 = DIRECTION ( 'NONE',  ( 0.000000000000000000, 0.000000000000000000, 1.000000000000000000 ) ) ;
#1212 = EDGE_CURVE ( 'NONE', #2036, #1136, #2120, .T. ) ;
#1213 = EDGE_CURVE ( 'NONE', #573, #758, #3350, .T. ) ;
#1214 = VECTOR ( 'NONE', #3440, 1000.000000000000000 ) ;
#1215 = DIRECTION ( 'NONE',  ( -0.000000000000000000, -0.5000000000000002220, 0.8660254037844384856 ) ) ;
#1216 = ORIENTED_EDGE ( 'NONE', *, *, #1000, .T. ) ;
#1217 = AXIS2_PLACEMENT_3D ( 'NONE', #349, #2733, #963 ) ;
#1218 = ORIENTED_EDGE ( 'NONE', *, *, #589, .T. ) ;
#1219 = DIRECTION ( 'NONE',  ( -1.000000000000000000, -0.000000000000000000, -0.000000000000000000 ) ) ;
#1220 = ORIENTED_EDGE ( 'NONE', *, *, #2326, .F. ) ;
#1221 = VECTOR ( 'NONE', #1981, 1000.000000000000114 ) ;
#1222 = DIRECTION ( 'NONE',  ( 0.000000000000000000, 0.000000000000000000, 1.000000000000000000 ) ) ;
#1223 = AXIS2_PLACEMENT_3D ( 'NONE', #3599, #935, #3286 ) ;
#1224 = ORIENTED_EDGE ( 'NONE', *, *, #2216, .F. ) ;
#1225 = DIRECTION ( 'NONE',  ( -1.000000000000000000, -0.000000000000000000, -0.000000000000000000 ) ) ;
#1226 = DIRECTION ( 'NONE',  ( -1.000000000000000000, 0.000000000000000000, 0.000000000000000000 ) ) ;
#1227 = SURFACE_STYLE_USAGE ( .BOTH. , #1789 ) ;
#1228 = DIRECTION ( 'NONE',  ( 1.241531209392323001E-18, 5.843967824224479992E-17, -1.000000000000000000 ) ) ;
#1229 = CLOSED_SHELL ( 'NONE', ( #776, #1258, #1235, #177, #1944, #1144, #2674, #3048, #1994, #110, #2461 ) ) ;
#1230 = DIRECTION ( 'NONE',  ( -1.000000000000000000, 0.000000000000000000, 0.000000000000000000 ) ) ;
#1231 = DIRECTION ( 'NONE',  ( -1.000000000000000000, 0.000000000000000000, 0.000000000000000000 ) ) ;
#1232 = PRODUCT_DEFINITION ( 'UNKNOWN', '', #3270, #1246 ) ;
#1233 = DIRECTION ( 'NONE',  ( 1.000000000000000000, 0.000000000000000000, 0.000000000000000000 ) ) ;
#1234 = VERTEX_POINT ( 'NONE', #1537 ) ;
#1235 = ADVANCED_FACE ( 'NONE', ( #877 ), #2964, .F. ) ;
#1236 = ORIENTED_EDGE ( 'NONE', *, *, #1776, .T. ) ;
#1237 = PLANE ( 'NONE',  #3384 ) ;
#1238 = VERTEX_POINT ( 'NONE', #998 ) ;
#1239 = DIRECTION ( 'NONE',  ( -1.000000000000000000, 0.000000000000000000, 0.000000000000000000 ) ) ;
#1240 = ADVANCED_FACE ( 'NONE', ( #1864 ), #2455, .T. ) ;
#1241 = ORIENTED_EDGE ( 'NONE', *, *, #546, .T. ) ;
#1242 = CARTESIAN_POINT ( 'NONE',  ( 0.000000000000000000, 0.000000000000000000, 1.102182119232617788E-16 ) ) ;
#1243 = DIRECTION ( 'NONE',  ( -0.000000000000000000, 0.4999999999999998890, -0.8660254037844387076 ) ) ;
#1244 = CARTESIAN_POINT ( 'NONE',  ( -82.50000000000000000, 19.84313483298442193, 0.000000000000000000 ) ) ;
#1245 = EDGE_CURVE ( 'NONE', #3752, #748, #786, .T. ) ;
#1246 = PRODUCT_DEFINITION_CONTEXT ( 'detailed design', #1566, 'design' ) ;
#1247 = LINE ( 'NONE', #3248, #3767 ) ;
#1248 = DIRECTION ( 'NONE',  ( -1.000000000000000000, 0.000000000000000000, -0.000000000000000000 ) ) ;
#1249 = DIRECTION ( 'NONE',  ( -1.000000000000000000, -0.000000000000000000, -0.000000000000000000 ) ) ;
#1250 = DIRECTION ( 'NONE',  ( 0.000000000000000000, 0.5000000000000001110, -0.8660254037844385966 ) ) ;
#1251 = EDGE_CURVE ( 'NONE', #3822, #2947, #3311, .T. ) ;
#1252 = ADVANCED_FACE ( 'NONE', ( #380 ), #362, .T. ) ;
#1253 = EDGE_LOOP ( 'NONE', ( #3192, #1444 ) ) ;
#1255 = VERTEX_POINT ( 'NONE', #1288 ) ;
#1254 = EDGE_CURVE ( 'NONE', #1889, #3067, #1834, .T. ) ;
#1256 = DIRECTION ( 'NONE',  ( -1.000000000000000000, -0.000000000000000000, -0.000000000000000000 ) ) ;
#1257 = VECTOR ( 'NONE', #2323, 1000.000000000000114 ) ;
#1258 = ADVANCED_FACE ( 'NONE', ( #2744 ), #1594, .F. ) ;
#1259 = EDGE_CURVE ( 'NONE', #910, #1798, #3531, .T. ) ;
#1260 = ORIENTED_EDGE ( 'NONE', *, *, #1698, .T. ) ;
#1261 = DIRECTION ( 'NONE',  ( 1.000000000000000000, 0.000000000000000000, -0.000000000000000000 ) ) ;
#1262 = CARTESIAN_POINT ( 'NONE',  ( -85.00000000000000000, 6.123233995736770227E-16, -5.000000000000000000 ) ) ;
#1263 = LINE ( 'NONE', #3347, #2938 ) ;
#1264 = VECTOR ( 'NONE', #2692, 1000.000000000000000 ) ;
#1265 = CIRCLE ( 'NONE', #3441, 22.50000000000000355 ) ;
#1266 = CARTESIAN_POINT ( 'NONE',  ( 1.600000000000000089, 8.572527594031473190E-16, -7.000000000000000000 ) ) ;
#1267 = PLANE ( 'NONE',  #1012 ) ;
#1268 = AXIS2_PLACEMENT_3D ( 'NONE', #310, #2992, #1500 ) ;
#1269 =( GEOMETRIC_REPRESENTATION_CONTEXT ( 3 ) GLOBAL_UNCERTAINTY_ASSIGNED_CONTEXT ( ( #3501 ) ) GLOBAL_UNIT_ASSIGNED_CONTEXT ( ( #2407, #572, #1760 ) ) REPRESENTATION_CONTEXT ( 'NONE', 'WORKASPACE' ) );
#1270 = DIRECTION ( 'NONE',  ( 0.000000000000000000, 0.8660254037844387076, -0.4999999999999999445 ) ) ;
#1271 = CARTESIAN_POINT ( 'NONE',  ( 1.300000000000000044, 0.7216878364870329410, 1.249999999999999778 ) ) ;
#1272 = AXIS2_PLACEMENT_3D ( 'NONE', #2214, #3715, #1563 ) ;
#1273 = ORIENTED_EDGE ( 'NONE', *, *, #930, .T. ) ;
#1274 = EDGE_CURVE ( 'NONE', #2771, #611, #3236, .T. ) ;
#1275 = ORIENTED_EDGE ( 'NONE', *, *, #3443, .T. ) ;
#1276 = CARTESIAN_POINT ( 'NONE',  ( -80.00000000000000000, 0.000000000000000000, 3.000000000000000000 ) ) ;
#1277 = CIRCLE ( 'NONE', #273, 25.15000000000000213 ) ;
#1278 = PRESENTATION_LAYER_ASSIGNMENT (  '', '', ( #2963 ) ) ;
#1279 = AXIS2_PLACEMENT_3D ( 'NONE', #3641, #2163, #1885 ) ;
#1280 = CARTESIAN_POINT ( 'NONE',  ( 0.000000000000000000, -1.443375672974063884, -3.691112476943992763E-18 ) ) ;
#1281 = VERTEX_POINT ( 'NONE', #277 ) ;
#1282 = CARTESIAN_POINT ( 'NONE',  ( -3.749999999999998224, -29.76470224947664533, -30.00000000000000000 ) ) ;
#1283 = DIRECTION ( 'NONE',  ( -0.000000000000000000, -1.000000000000000000, -0.000000000000000000 ) ) ;
#1284 = EDGE_CURVE ( 'NONE', #261, #1954, #1523, .T. ) ;
#1285 = VECTOR ( 'NONE', #3099, 999.9999999999998863 ) ;
#1286 = CARTESIAN_POINT ( 'NONE',  ( -70.00000000000000000, 0.000000000000000000, -4.999999999999997335 ) ) ;
#1287 = CARTESIAN_POINT ( 'NONE',  ( 4.336808689942017736E-16, 0.000000000000000000, 0.000000000000000000 ) ) ;
#1288 = CARTESIAN_POINT ( 'NONE',  ( 11.80999999999999872, 2.449293598294705921E-16, -1.999999999999999556 ) ) ;
#1289 = CARTESIAN_POINT ( 'NONE',  ( 0.000000000000000000, 0.000000000000000000, -30.00000000000000000 ) ) ;
#1290 = ADVANCED_FACE ( 'NONE', ( #3603 ), #3028, .F. ) ;
#1291 = ORIENTED_EDGE ( 'NONE', *, *, #347, .F. ) ;
#1292 = CARTESIAN_POINT ( 'NONE',  ( -80.00000000000000000, 0.000000000000000000, -5.000000000000000000 ) ) ;
#1293 = ORIENTED_EDGE ( 'NONE', *, *, #2111, .F. ) ;
#1294 = PLANE ( 'NONE',  #450 ) ;
#1295 = EDGE_CURVE ( 'NONE', #2309, #1351, #2897, .T. ) ;
#1296 = CARTESIAN_POINT ( 'NONE',  ( 2.199999999999999734, 0.000000000000000000, 2.199999999999999289 ) ) ;
#1297 = ORIENTED_EDGE ( 'NONE', *, *, #2658, .T. ) ;
#1298 = CARTESIAN_POINT ( 'NONE',  ( 0.000000000000000000, 0.000000000000000000, -24.00000000000000000 ) ) ;
#1299 = PLANE ( 'NONE',  #393 ) ;
#1300 = DIRECTION ( 'NONE',  ( 0.000000000000000000, 0.000000000000000000, 1.000000000000000000 ) ) ;
#1301 = LINE ( 'NONE', #677, #3821 ) ;
#1302 = VERTEX_POINT ( 'NONE', #744 ) ;
#1303 = DIRECTION ( 'NONE',  ( 0.000000000000000000, 0.000000000000000000, 1.000000000000000000 ) ) ;
#1304 = ADVANCED_FACE ( 'NONE', ( #1386 ), #2554, .T. ) ;
#1305 = FACE_OUTER_BOUND ( 'NONE', #2952, .T. ) ;
#1306 = CARTESIAN_POINT ( 'NONE',  ( 0.000000000000000000, 0.000000000000000000, 0.000000000000000000 ) ) ;
#1307 = ORIENTED_EDGE ( 'NONE', *, *, #3136, .T. ) ;
#1308 =( LENGTH_UNIT ( ) NAMED_UNIT ( * ) SI_UNIT ( .MILLI., .METRE. ) );
#1309 = ORIENTED_EDGE ( 'NONE', *, *, #2920, .T. ) ;
#1310 = LINE ( 'NONE', #2206, #1706 ) ;
#1311 = LINE ( 'NONE', #101, #2818 ) ;
#1312 = ORIENTED_EDGE ( 'NONE', *, *, #970, .F. ) ;
#1313 = CARTESIAN_POINT ( 'NONE',  ( 0.000000000000000000, 0.000000000000000000, 5.000000000000000000 ) ) ;
#1314 = CARTESIAN_POINT ( 'NONE',  ( 1.300000000000000044, 0.7216878364870329410, -1.250000000000000000 ) ) ;
#1315 = CIRCLE ( 'NONE', #2746, 2.000000000000001776 ) ;
#1316 = AXIS2_PLACEMENT_3D ( 'NONE', #501, #3743, #2848 ) ;
#1317 = DIRECTION ( 'NONE',  ( 0.000000000000000000, 0.000000000000000000, 1.000000000000000000 ) ) ;
#1318 = ORIENTED_EDGE ( 'NONE', *, *, #3095, .T. ) ;
#1319 = FACE_OUTER_BOUND ( 'NONE', #3009, .T. ) ;
#1320 = AXIS2_PLACEMENT_3D ( 'NONE', #595, #1194, #3572 ) ;
#1321 = AXIS2_PLACEMENT_3D ( 'NONE', #228, #541, #210 ) ;
#1322 = APPLICATION_PROTOCOL_DEFINITION ( 'draft international standard', 'automotive_design', 1998, #3024 ) ;
#1323 = CIRCLE ( 'NONE', #1633, 4.499999999999993783 ) ;
#1324 = VECTOR ( 'NONE', #798, 1000.000000000000114 ) ;
#1325 = DIRECTION ( 'NONE',  ( 1.000000000000000000, 0.000000000000000000, 0.000000000000000000 ) ) ;
#1326 = CARTESIAN_POINT ( 'NONE',  ( 1.300000000000000044, -0.7216878364870318308, 1.249999999999999778 ) ) ;
#1327 = EDGE_CURVE ( 'NONE', #1, #1495, #2210, .T. ) ;
#1328 = AXIS2_PLACEMENT_3D ( 'NONE', #1585, #2545, #2479 ) ;
#1329 = ORIENTED_EDGE ( 'NONE', *, *, #145, .T. ) ;
#1330 = ORIENTED_EDGE ( 'NONE', *, *, #2686, .F. ) ;
#1331 = DIRECTION ( 'NONE',  ( -0.9921567416492215186, 0.1250000000000000833, 0.000000000000000000 ) ) ;
#1332 = FACE_OUTER_BOUND ( 'NONE', #2931, .T. ) ;
#1333 = ORIENTED_EDGE ( 'NONE', *, *, #3449, .T. ) ;
#1334 = CARTESIAN_POINT ( 'NONE',  ( 0.000000000000000000, 0.000000000000000000, 0.000000000000000000 ) ) ;
#1335 = CIRCLE ( 'NONE', #527, 3.799999999999999378 ) ;
#1336 = VECTOR ( 'NONE', #999, 1000.000000000000000 ) ;
#1337 = FACE_OUTER_BOUND ( 'NONE', #2966, .T. ) ;
#1338 = DIRECTION ( 'NONE',  ( 0.000000000000000000, 0.000000000000000000, -1.000000000000000000 ) ) ;
#1339 = EDGE_CURVE ( 'NONE', #2659, #688, #2201, .T. ) ;
#1340 = AXIS2_PLACEMENT_3D ( 'NONE', #839, #2026, #1432 ) ;
#1341 = FACE_OUTER_BOUND ( 'NONE', #3463, .T. ) ;
#1342 = CARTESIAN_POINT ( 'NONE',  ( 0.000000000000000000, 0.000000000000000000, -20.00000000000000000 ) ) ;
#1343 = DIRECTION ( 'NONE',  ( -1.000000000000000000, 0.000000000000000000, 0.000000000000000000 ) ) ;
#1344 = AXIS2_PLACEMENT_3D ( 'NONE', #2537, #3428, #2224 ) ;
#1345 = PRODUCT_DEFINITION_FORMATION_WITH_SPECIFIED_SOURCE ( 'ANY', '', #3397, .NOT_KNOWN. ) ;
#1346 = VERTEX_POINT ( 'NONE', #1927 ) ;
#1347 = PRODUCT_CONTEXT ( 'NONE', #781, 'mechanical' ) ;
#1348 = EDGE_CURVE ( 'NONE', #2909, #1784, #1840, .T. ) ;
#1349 = DIRECTION ( 'NONE',  ( 0.000000000000000000, -0.5000000000000000000, -0.8660254037844385966 ) ) ;
#1350 = CYLINDRICAL_SURFACE ( 'NONE', #3261, 3.799999999999999378 ) ;
#1351 = VERTEX_POINT ( 'NONE', #2801 ) ;
#1352 = LINE ( 'NONE', #1992, #2194 ) ;
#1353 = ORIENTED_EDGE ( 'NONE', *, *, #3202, .T. ) ;
#1354 = CARTESIAN_POINT ( 'NONE',  ( -3.750000000000004441, 29.76470224947664533, -30.00000000000000000 ) ) ;
#1355 = FACE_OUTER_BOUND ( 'NONE', #1118, .T. ) ;
#1356 = ORIENTED_EDGE ( 'NONE', *, *, #2359, .F. ) ;
#1357 = FACE_OUTER_BOUND ( 'NONE', #2852, .T. ) ;
#1358 = LINE ( 'NONE', #1649, #1214 ) ;
#1359 = CARTESIAN_POINT ( 'NONE',  ( 9.809999999999998721, 0.000000000000000000, 0.000000000000000000 ) ) ;
#1360 = ADVANCED_FACE ( 'NONE', ( #1612 ), #787, .T. ) ;
#1361 = ORIENTED_EDGE ( 'NONE', *, *, #388, .T. ) ;
#1362 = DIRECTION ( 'NONE',  ( -1.000000000000000000, 0.000000000000000000, 0.000000000000000000 ) ) ;
#1363 = LINE ( 'NONE', #1608, #3303 ) ;
#1364 =( NAMED_UNIT ( * ) SI_UNIT ( $, .STERADIAN. ) SOLID_ANGLE_UNIT ( ) );
#1365 = CYLINDRICAL_SURFACE ( 'NONE', #1077, 20.00000000000000355 ) ;
#1366 = ORIENTED_EDGE ( 'NONE', *, *, #2311, .F. ) ;
#1367 =( NAMED_UNIT ( * ) SI_UNIT ( $, .STERADIAN. ) SOLID_ANGLE_UNIT ( ) );
#1368 = VERTEX_POINT ( 'NONE', #2293 ) ;
#1369 = CIRCLE ( 'NONE', #1684, 1.610000000000000098 ) ;
#1370 = PLANE ( 'NONE',  #263 ) ;
#1371 = EDGE_CURVE ( 'NONE', #748, #2736, #1973, .T. ) ;
#1372 = UNCERTAINTY_MEASURE_WITH_UNIT (LENGTH_MEASURE( 1.000000000000000082E-05 ), #747, 'distance_accuracy_value', 'NONE');
#1373 = CARTESIAN_POINT ( 'NONE',  ( -82.50000000000000000, 19.84313483298442193, 5.000000000000000000 ) ) ;
#1374 = VERTEX_POINT ( 'NONE', #487 ) ;
#1375 = APPLICATION_CONTEXT ( 'automotive_design' ) ;
#1376 = CARTESIAN_POINT ( 'NONE',  ( 1.820000000000000062, 0.000000000000000000, 3.799999999999999378 ) ) ;
#1377 = DIRECTION ( 'NONE',  ( -0.000000000000000000, -0.000000000000000000, 1.000000000000000000 ) ) ;
#1378 = EDGE_CURVE ( 'NONE', #465, #2228, #3121, .T. ) ;
#1379 = EDGE_CURVE ( 'NONE', #929, #1408, #2496, .T. ) ;
#1380 = EDGE_LOOP ( 'NONE', ( #3293, #2842 ) ) ;
#1381 = LINE ( 'NONE', #1715, #1407 ) ;
#1382 = DIRECTION ( 'NONE',  ( -1.000000000000000000, 0.000000000000000000, 0.000000000000000000 ) ) ;
#1383 =( LENGTH_UNIT ( ) NAMED_UNIT ( * ) SI_UNIT ( .MILLI., .METRE. ) );
#1384 = AXIS2_PLACEMENT_3D ( 'NONE', #3193, #1720, #2904 ) ;
#1385 = APPLICATION_PROTOCOL_DEFINITION ( 'draft international standard', 'automotive_design', 1998, #1892 ) ;
#1386 = FACE_OUTER_BOUND ( 'NONE', #2322, .T. ) ;
#1387 = CIRCLE ( 'NONE', #3557, 18.99999999999999645 ) ;
#1388 = PRESENTATION_LAYER_ASSIGNMENT (  '', '', ( #257 ) ) ;
#1389 = CIRCLE ( 'NONE', #2195, 2.700000000000000178 ) ;
#1390 = EDGE_LOOP ( 'NONE', ( #2719, #2420, #1333, #2005, #1429 ) ) ;
#1391 = FACE_OUTER_BOUND ( 'NONE', #309, .T. ) ;
#1392 = VERTEX_POINT ( 'NONE', #3762 ) ;
#1393 = CIRCLE ( 'NONE', #2132, 2.000000000000000000 ) ;
#1394 = DIRECTION ( 'NONE',  ( 1.000000000000000000, 0.000000000000000000, 0.000000000000000000 ) ) ;
#1395 = ORIENTED_EDGE ( 'NONE', *, *, #1571, .F. ) ;
#1396 = LINE ( 'NONE', #3790, #1041 ) ;
#1397 = CARTESIAN_POINT ( 'NONE',  ( 1.600000000000000089, 0.000000000000000000, 0.000000000000000000 ) ) ;
#1398 = ORIENTED_EDGE ( 'NONE', *, *, #2612, .T. ) ;
#1399 = DIRECTION ( 'NONE',  ( -0.000000000000000000, -0.000000000000000000, 1.000000000000000000 ) ) ;
#1400 = FILL_AREA_STYLE ('',( #2372 ) ) ;
#1401 =( LENGTH_UNIT ( ) NAMED_UNIT ( * ) SI_UNIT ( .MILLI., .METRE. ) );
#1402 = CIRCLE ( 'NONE', #1404, 3.799999999999999378 ) ;
#1403 = UNCERTAINTY_MEASURE_WITH_UNIT (LENGTH_MEASURE( 1.000000000000000082E-05 ), #953, 'distance_accuracy_value', 'NONE');
#1404 = AXIS2_PLACEMENT_3D ( 'NONE', #737, #3074, #2777 ) ;
#1405 = FACE_OUTER_BOUND ( 'NONE', #768, .T. ) ;
#1406 = ADVANCED_FACE ( 'NONE', ( #2861 ), #1192, .F. ) ;
#1407 = VECTOR ( 'NONE', #540, 1000.000000000000000 ) ;
#1408 = VERTEX_POINT ( 'NONE', #2882 ) ;
#1409 = ORIENTED_EDGE ( 'NONE', *, *, #2491, .T. ) ;
#1410 = EDGE_CURVE ( 'NONE', #2092, #1873, #1871, .T. ) ;
#1411 = DIRECTION ( 'NONE',  ( -1.000000000000000000, 0.000000000000000000, 0.000000000000000000 ) ) ;
#1412 = ORIENTED_EDGE ( 'NONE', *, *, #1811, .F. ) ;
#1413 = CARTESIAN_POINT ( 'NONE',  ( 2.200000000000000178, 4.653657836759941744E-16, -3.799999999999999378 ) ) ;
#1414 = CARTESIAN_POINT ( 'NONE',  ( 0.000000000000000000, -0.7216878364870317197, -1.250000000000000000 ) ) ;
#1415 = ORIENTED_EDGE ( 'NONE', *, *, #2974, .T. ) ;
#1416 = DIRECTION ( 'NONE',  ( -1.000000000000000000, -0.000000000000000000, -0.000000000000000000 ) ) ;
#1417 = CYLINDRICAL_SURFACE ( 'NONE', #1321, 5.000000000000004441 ) ;
#1418 = ORIENTED_EDGE ( 'NONE', *, *, #2998, .T. ) ;
#1419 = ADVANCED_FACE ( 'NONE', ( #1305 ), #2489, .T. ) ;
#1420 = CARTESIAN_POINT ( 'NONE',  ( 12.20000000000000107, 0.000000000000000000, 1.610000000000000098 ) ) ;
#1421 = APPLICATION_CONTEXT ( 'automotive_design' ) ;
#1422 = ADVANCED_FACE ( 'NONE', ( #2512 ), #1910, .F. ) ;
#1423 = DIRECTION ( 'NONE',  ( -0.000000000000000000, 0.000000000000000000, 1.000000000000000000 ) ) ;
#1424 = ORIENTED_EDGE ( 'NONE', *, *, #2738, .T. ) ;
#1425 = DIRECTION ( 'NONE',  ( 0.3361233252211006661, -0.8797966926992965009, -0.3361233252211005551 ) ) ;
#1426 = ORIENTED_EDGE ( 'NONE', *, *, #2738, .F. ) ;
#1427 = DIRECTION ( 'NONE',  ( -0.9921567416492214075, 0.1250000000000000555, 0.000000000000000000 ) ) ;
#1428 = CARTESIAN_POINT ( 'NONE',  ( -80.00000000000000000, 0.000000000000000000, -4.999999999999997335 ) ) ;
#1429 = ORIENTED_EDGE ( 'NONE', *, *, #34, .F. ) ;
#1430 = DIRECTION ( 'NONE',  ( 0.000000000000000000, 0.000000000000000000, 1.000000000000000000 ) ) ;
#1431 = DIRECTION ( 'NONE',  ( -1.795453617517838654E-17, 1.015442787603507153E-17, 1.000000000000000000 ) ) ;
#1432 = DIRECTION ( 'NONE',  ( 0.9219985364506716463, -0.3871933609746164295, -1.068005703307140349E-17 ) ) ;
#1433 = EDGE_LOOP ( 'NONE', ( #2166, #592, #1418 ) ) ;
#1434 = PLANE ( 'NONE',  #2376 ) ;
#1435 = VECTOR ( 'NONE', #2049, 1000.000000000000000 ) ;
#1436 = ADVANCED_FACE ( 'NONE', ( #3107 ), #1365, .T. ) ;
#1437 = AXIS2_PLACEMENT_3D ( 'NONE', #520, #227, #498 ) ;
#1438 = DIRECTION ( 'NONE',  ( -0.9921567416492214075, 0.1250000000000000555, 0.000000000000000000 ) ) ;
#1439 = ORIENTED_EDGE ( 'NONE', *, *, #317, .F. ) ;
#1440 = CIRCLE ( 'NONE', #2569, 2.700000000000000178 ) ;
#1441 = AXIS2_PLACEMENT_3D ( 'NONE', #891, #2663, #652 ) ;
#1442 = EDGE_LOOP ( 'NONE', ( #1318, #2099 ) ) ;
#1443 = CARTESIAN_POINT ( 'NONE',  ( 1.300000000000000044, 0.000000000000000000, 0.000000000000000000 ) ) ;
#1444 = ORIENTED_EDGE ( 'NONE', *, *, #2111, .T. ) ;
#1445 = DIRECTION ( 'NONE',  ( -0.000000000000000000, -0.000000000000000000, -1.000000000000000000 ) ) ;
#1446 = CIRCLE ( 'NONE', #3012, 2.000000000000000000 ) ;
#1447 = CARTESIAN_POINT ( 'NONE',  ( -90.00000000000000000, 0.000000000000000000, -30.00000000000000000 ) ) ;
#1448 = CIRCLE ( 'NONE', #3371, 18.99999999999999645 ) ;
#1449 = PRODUCT_CONTEXT ( 'NONE', #1892, 'mechanical' ) ;
#1450 = ORIENTED_EDGE ( 'NONE', *, *, #1259, .T. ) ;
#1451 = CARTESIAN_POINT ( 'NONE',  ( -20.00000000000000000, 2.449293598294706513E-15, 0.000000000000000000 ) ) ;
#1452 = DIRECTION ( 'NONE',  ( 0.000000000000000000, 1.000000000000000000, 0.000000000000000000 ) ) ;
#1453 = PRESENTATION_STYLE_ASSIGNMENT (( #229 ) ) ;
#1454 = ORIENTED_EDGE ( 'NONE', *, *, #3508, .F. ) ;
#1455 = CARTESIAN_POINT ( 'NONE',  ( 1.300000000000000044, -1.082531754730548412, -0.6250000000000003331 ) ) ;
#1456 = CARTESIAN_POINT ( 'NONE',  ( -997.9783121635130101, 0.000000000000000000, 0.000000000000000000 ) ) ;
#1457 = CIRCLE ( 'NONE', #3637, 30.00000000000000000 ) ;
#1458 = ADVANCED_FACE ( 'NONE', ( #155 ), #3142, .T. ) ;
#1459 = MECHANICAL_DESIGN_GEOMETRIC_PRESENTATION_REPRESENTATION (  '', ( #2338 ), #1836 ) ;
#1460 = AXIS2_PLACEMENT_3D ( 'NONE', #1741, #1445, #2314 ) ;
#1461 = DIRECTION ( 'NONE',  ( 0.000000000000000000, 0.000000000000000000, -1.000000000000000000 ) ) ;
#1462 = ORIENTED_EDGE ( 'NONE', *, *, #750, .F. ) ;
#1463 = AXIS2_PLACEMENT_3D ( 'NONE', #3018, #3597, #1803 ) ;
#1464 = EDGE_LOOP ( 'NONE', ( #235, #3768, #239, #596 ) ) ;
#1465 = DIRECTION ( 'NONE',  ( -1.000000000000000000, 0.000000000000000000, -0.000000000000000000 ) ) ;
#1466 = EDGE_LOOP ( 'NONE', ( #2807, #2915, #3512, #118, #3164 ) ) ;
#1467 = CARTESIAN_POINT ( 'NONE',  ( -80.00000000000000000, 0.000000000000000000, -30.00000000000000000 ) ) ;
#1468 = DIRECTION ( 'NONE',  ( -0.000000000000000000, -0.000000000000000000, -1.000000000000000000 ) ) ;
#1469 = ORIENTED_EDGE ( 'NONE', *, *, #516, .T. ) ;
#1470 = CARTESIAN_POINT ( 'NONE',  ( -82.00000000000000000, 0.000000000000000000, -5.000000000000000000 ) ) ;
#1471 = CARTESIAN_POINT ( 'NONE',  ( -20.00000000000000000, 2.449293598294706513E-15, -20.00000000000000000 ) ) ;
#1472 = DIRECTION ( 'NONE',  ( 0.000000000000000000, 0.000000000000000000, -1.000000000000000000 ) ) ;
#1473 =( NAMED_UNIT ( * ) PLANE_ANGLE_UNIT ( ) SI_UNIT ( $, .RADIAN. ) );
#1474 = ORIENTED_EDGE ( 'NONE', *, *, #1626, .F. ) ;
#1475 = FACE_OUTER_BOUND ( 'NONE', #252, .T. ) ;
#1476 = CARTESIAN_POINT ( 'NONE',  ( 1.300000000000000044, 1.082531754730548856, 0.6250000000000006661 ) ) ;
#1477 = CARTESIAN_POINT ( 'NONE',  ( 12.20000000000000107, 0.000000000000000000, 0.000000000000000000 ) ) ;
#1478 = VERTEX_POINT ( 'NONE', #1476 ) ;
#1479 = ORIENTED_EDGE ( 'NONE', *, *, #2634, .F. ) ;
#1480 = EDGE_CURVE ( 'NONE', #447, #2912, #2805, .T. ) ;
#1481 = CARTESIAN_POINT ( 'NONE',  ( 12.20000000000000107, 0.000000000000000000, 1.610000000000000098 ) ) ;
#1482 = ORIENTED_EDGE ( 'NONE', *, *, #2447, .F. ) ;
#1483 = DIRECTION ( 'NONE',  ( -1.000000000000000000, 0.000000000000000000, 0.000000000000000000 ) ) ;
#1484 = ITEM_DEFINED_TRANSFORMATION ( 'NONE', 'NONE', #1722,  #2207 ) ;
#1485 = EDGE_LOOP ( 'NONE', ( #3595, #249, #1671, #2789 ) ) ;
#1486 = CARTESIAN_POINT ( 'NONE',  ( 2.400000000000000799, 0.000000000000000000, 0.000000000000000000 ) ) ;
#1487 = LINE ( 'NONE', #1588, #789 ) ;
#1488 = ADVANCED_FACE ( 'NONE', ( #2342 ), #2942, .F. ) ;
#1489 = EDGE_CURVE ( 'NONE', #1105, #3089, #842, .T. ) ;
#1490 = ORIENTED_EDGE ( 'NONE', *, *, #3224, .T. ) ;
#1491 = DIRECTION ( 'NONE',  ( -1.000000000000000000, 0.000000000000000000, 0.000000000000000000 ) ) ;
#1492 = DIRECTION ( 'NONE',  ( -1.000000000000000000, -0.000000000000000000, -0.000000000000000000 ) ) ;
#1493 = DIRECTION ( 'NONE',  ( 0.000000000000000000, 0.000000000000000000, 1.000000000000000000 ) ) ;
#1494 = LINE ( 'NONE', #591, #2943 ) ;
#1495 = VERTEX_POINT ( 'NONE', #2032 ) ;
#1496 = AXIS2_PLACEMENT_3D ( 'NONE', #321, #1969, #724 ) ;
#1497 = ORIENTED_EDGE ( 'NONE', *, *, #3426, .F. ) ;
#1498 = DIRECTION ( 'NONE',  ( -0.000000000000000000, 0.000000000000000000, 1.000000000000000000 ) ) ;
#1499 = ORIENTED_EDGE ( 'NONE', *, *, #1245, .F. ) ;
#1500 = DIRECTION ( 'NONE',  ( -0.000000000000000000, 0.000000000000000000, -1.000000000000000000 ) ) ;
#1501 = AXIS2_PLACEMENT_3D ( 'NONE', #3243, #881, #3227 ) ;
#1502 = VECTOR ( 'NONE', #647, 1000.000000000000000 ) ;
#1503 = CIRCLE ( 'NONE', #2570, 18.99999999999999645 ) ;
#1504 = ORIENTED_EDGE ( 'NONE', *, *, #3613, .T. ) ;
#1505 = FACE_OUTER_BOUND ( 'NONE', #3214, .T. ) ;
#1506 = PLANE ( 'NONE',  #3764 ) ;
#1507 = DIRECTION ( 'NONE',  ( -0.000000000000000000, -0.000000000000000000, -1.000000000000000000 ) ) ;
#1508 = DIRECTION ( 'NONE',  ( 0.4874982642792389242, -0.8731239558760996999, -5.041983873736794523E-17 ) ) ;
#1509 = CIRCLE ( 'NONE', #3756, 1.999999999999999112 ) ;
#1510 = DIRECTION ( 'NONE',  ( -1.000000000000000000, -0.000000000000000000, -0.000000000000000000 ) ) ;
#1511 = CIRCLE ( 'NONE', #1953, 30.00000000000000000 ) ;
#1512 = DIRECTION ( 'NONE',  ( -0.000000000000000000, -0.000000000000000000, -1.000000000000000000 ) ) ;
#1513 = AXIS2_PLACEMENT_3D ( 'NONE', #320, #3560, #3601 ) ;
#1514 = ADVANCED_FACE ( 'NONE', ( #3215 ), #7, .F. ) ;
#1515 = DIRECTION ( 'NONE',  ( -1.000000000000000000, 0.000000000000000000, 0.000000000000000000 ) ) ;
#1516 = VERTEX_POINT ( 'NONE', #3798 ) ;
#1517 = CIRCLE ( 'NONE', #3636, 1.324999999999999734 ) ;
#1518 = AXIS2_PLACEMENT_3D ( 'NONE', #1334, #144, #168 ) ;
#1519 = ORIENTED_EDGE ( 'NONE', *, *, #206, .T. ) ;
#1520 = SURFACE_STYLE_FILL_AREA ( #1838 ) ;
#1521 = EDGE_LOOP ( 'NONE', ( #1454, #2845, #2307, #2636 ) ) ;
#1522 = MECHANICAL_DESIGN_GEOMETRIC_PRESENTATION_REPRESENTATION (  '', ( #2963 ), #1154 ) ;
#1523 = CIRCLE ( 'NONE', #1899, 9.999999999999994671 ) ;
#1524 = CARTESIAN_POINT ( 'NONE',  ( 1.820000000000000062, -3.800000000000000266, -4.653657836759940757E-16 ) ) ;
#1525 = EDGE_CURVE ( 'NONE', #3210, #1889, #3541, .T. ) ;
#1526 = ADVANCED_BREP_SHAPE_REPRESENTATION ( '', ( #3253, #2207 ), #2713 ) ;
#1527 = AXIS2_PLACEMENT_3D ( 'NONE', #39, #2997, #619 ) ;
#1528 = VERTEX_POINT ( 'NONE', #588 ) ;
#1529 = DIRECTION ( 'NONE',  ( -0.000000000000000000, -0.000000000000000000, -1.000000000000000000 ) ) ;
#1530 = DIRECTION ( 'NONE',  ( -1.000000000000000000, -0.000000000000000000, -0.000000000000000000 ) ) ;
#1531 = CARTESIAN_POINT ( 'NONE',  ( 1.300000000000000044, -1.443375672974064328, 1.278502688459867223E-18 ) ) ;
#1532 = EDGE_CURVE ( 'NONE', #821, #2587, #869, .T. ) ;
#1533 = EDGE_CURVE ( 'NONE', #2771, #1105, #251, .T. ) ;
#1534 = PLANE ( 'NONE',  #696 ) ;
#1535 = ADVANCED_FACE ( 'NONE', ( #1405 ), #212, .T. ) ;
#1536 = EDGE_CURVE ( 'NONE', #1392, #3277, #3249, .T. ) ;
#1537 = CARTESIAN_POINT ( 'NONE',  ( -70.00000000000000000, 0.000000000000000000, -4.999999999999997335 ) ) ;
#1538 = DIRECTION ( 'NONE',  ( -1.000000000000000000, 0.000000000000000000, 0.000000000000000000 ) ) ;
#1539 = ADVANCED_FACE ( 'NONE', ( #1131 ), #1152, .T. ) ;
#1540 = EDGE_CURVE ( 'NONE', #3277, #3156, #3504, .T. ) ;
#1541 = CLOSED_SHELL ( 'NONE', ( #278, #1925, #2926, #1539, #3829, #955, #1733, #1863, #2069, #237, #2630, #1240, #1514, #2999, #1186, #685, #1669, #3042, #3370, #467, #3195, #981, #2731, #1806, #2222, #2555, #1582 ) ) ;
#1542 = VERTEX_POINT ( 'NONE', #1116 ) ;
#1543 = DIRECTION ( 'NONE',  ( 1.000000000000000000, 0.000000000000000000, 0.000000000000000000 ) ) ;
#1544 = VERTEX_POINT ( 'NONE', #1774 ) ;
#1545 = LINE ( 'NONE', #2737, #1946 ) ;
#1546 = ORIENTED_EDGE ( 'NONE', *, *, #2251, .F. ) ;
#1547 = CARTESIAN_POINT ( 'NONE',  ( 0.000000000000000000, 0.000000000000000000, -20.00000000000000000 ) ) ;
#1548 = LINE ( 'NONE', #675, #2274 ) ;
#1549 = DIRECTION ( 'NONE',  ( -1.000000000000000000, 0.000000000000000000, 0.000000000000000000 ) ) ;
#1550 = CARTESIAN_POINT ( 'NONE',  ( -85.00000000000000000, 0.000000000000000000, -4.999999999999997335 ) ) ;
#1551 = LINE ( 'NONE', #2139, #2004 ) ;
#1552 = ADVANCED_FACE ( 'NONE', ( #1749, #247 ), #1434, .T. ) ;
#1553 = CARTESIAN_POINT ( 'NONE',  ( 0.000000000000000000, 0.000000000000000000, 0.000000000000000000 ) ) ;
#1554 = CARTESIAN_POINT ( 'NONE',  ( 0.000000000000000000, 0.000000000000000000, 0.000000000000000000 ) ) ;
#1555 = ORIENTED_EDGE ( 'NONE', *, *, #2618, .F. ) ;
#1556 = SURFACE_STYLE_FILL_AREA ( #365 ) ;
#1557 = ORIENTED_EDGE ( 'NONE', *, *, #740, .T. ) ;
#1558 = DIRECTION ( 'NONE',  ( 0.1250000000000001665, -0.9921567416492215186, 0.000000000000000000 ) ) ;
#1559 = AXIS2_PLACEMENT_3D ( 'NONE', #1287, #3305, #2689 ) ;
#1560 = CARTESIAN_POINT ( 'NONE',  ( -3.750000000000004441, 29.76470224947664533, 0.000000000000000000 ) ) ;
#1561 = ORIENTED_EDGE ( 'NONE', *, *, #2401, .T. ) ;
#1562 = DIRECTION ( 'NONE',  ( -0.000000000000000000, 0.000000000000000000, 1.000000000000000000 ) ) ;
#1563 = DIRECTION ( 'NONE',  ( 0.000000000000000000, 0.000000000000000000, 1.000000000000000000 ) ) ;
#1564=STYLED_ITEM('',(#3860),#1966);
#1565 = SURFACE_STYLE_USAGE ( .BOTH. , #373 ) ;
#1566 = APPLICATION_CONTEXT ( 'automotive_design' ) ;
#1567 = VECTOR ( 'NONE', #670, 1000.000000000000114 ) ;
#1568 = CARTESIAN_POINT ( 'NONE',  ( 0.000000000000000000, 0.7216878364870328300, -1.250000000000000000 ) ) ;
#1569 = DIRECTION ( 'NONE',  ( -1.000000000000000000, 0.000000000000000000, -0.000000000000000000 ) ) ;
#1570 = AXIS2_PLACEMENT_3D ( 'NONE', #313, #2724, #2370 ) ;
#1571 = EDGE_CURVE ( 'NONE', #868, #916, #3242, .T. ) ;
#1572 = ADVANCED_BREP_SHAPE_REPRESENTATION ( '', ( #3213, #2207 ), #2896 ) ;
#1573 = DIRECTION ( 'NONE',  ( 1.000000000000000000, 0.000000000000000000, 0.000000000000000000 ) ) ;
#1574 = CARTESIAN_POINT ( 'NONE',  ( 30.00000000000000000, 0.000000000000000000, -30.00000000000000000 ) ) ;
#1575 = EDGE_CURVE ( 'NONE', #1495, #137, #232, .T. ) ;
#1576 = CIRCLE ( 'NONE', #2459, 1.610000000000000098 ) ;
#1577 = VERTEX_POINT ( 'NONE', #3230 ) ;
#1578 = FILL_AREA_STYLE_COLOUR ( '', #1138 ) ;
#1579 = ORIENTED_EDGE ( 'NONE', *, *, #2292, .F. ) ;
#1580 = DIRECTION ( 'NONE',  ( -1.000000000000000000, 0.000000000000000000, 0.000000000000000000 ) ) ;
#1581 = AXIS2_PLACEMENT_3D ( 'NONE', #2728, #2672, #1491 ) ;
#1582 = ADVANCED_FACE ( 'NONE', ( #267 ), #193, .F. ) ;
#1583 = MECHANICAL_DESIGN_GEOMETRIC_PRESENTATION_REPRESENTATION (  '', ( #1651 ), #2089 ) ;
#1584 = AXIS2_PLACEMENT_3D ( 'NONE', #3222, #2581, #3154 ) ;
#1585 = CARTESIAN_POINT ( 'NONE',  ( 3.885274725274725949, -4.336808689942017736E-16, 0.000000000000000000 ) ) ;
#1586 = EDGE_LOOP ( 'NONE', ( #1592, #3789, #2611, #3671, #3173 ) ) ;
#1587 = DIRECTION ( 'NONE',  ( 0.000000000000000000, 1.000000000000000000, 0.000000000000000000 ) ) ;
#1588 = CARTESIAN_POINT ( 'NONE',  ( 2.021687836487040535, 2.655529440325959183E-32, -2.168404344971008868E-16 ) ) ;
#1589 = PLANE ( 'NONE',  #3310 ) ;
#1590 = AXIS2_PLACEMENT_3D ( 'NONE', #2501, #2529, #1903 ) ;
#1591 = DIRECTION ( 'NONE',  ( 0.000000000000000000, -0.000000000000000000, -1.000000000000000000 ) ) ;
#1592 = ORIENTED_EDGE ( 'NONE', *, *, #191, .T. ) ;
#1593 = DIRECTION ( 'NONE',  ( 0.9921567416492215186, 0.1250000000000001665, 0.000000000000000000 ) ) ;
#1594 = CYLINDRICAL_SURFACE ( 'NONE', #1652, 1.649999999999999245 ) ;
#1595 = FACE_OUTER_BOUND ( 'NONE', #1801, .T. ) ;
#1596 = ORIENTED_EDGE ( 'NONE', *, *, #2658, .F. ) ;
#1597 =( NAMED_UNIT ( * ) PLANE_ANGLE_UNIT ( ) SI_UNIT ( $, .RADIAN. ) );
#1598 = VERTEX_POINT ( 'NONE', #1861 ) ;
#1599 = DIRECTION ( 'NONE',  ( -0.000000000000000000, 0.000000000000000000, -1.000000000000000000 ) ) ;
#1600 = DIRECTION ( 'NONE',  ( -1.000000000000000000, -0.000000000000000000, -0.000000000000000000 ) ) ;
#1601 = ORIENTED_EDGE ( 'NONE', *, *, #2388, .T. ) ;
#1602 = PLANE ( 'NONE',  #3454 ) ;
#1603 = CARTESIAN_POINT ( 'NONE',  ( -3.750000000000004441, 29.76470224947664533, 0.000000000000000000 ) ) ;
#1604 = DIRECTION ( 'NONE',  ( -1.000000000000000000, 0.000000000000000000, -0.000000000000000000 ) ) ;
#1605 = ADVANCED_FACE ( 'NONE', ( #2119, #2709 ), #2729, .T. ) ;
#1606 = LINE ( 'NONE', #1922, #3206 ) ;
#1607 = ORIENTED_EDGE ( 'NONE', *, *, #1378, .F. ) ;
#1608 = CARTESIAN_POINT ( 'NONE',  ( -20.00000000000000000, 2.449293598294706513E-15, -20.00000000000000000 ) ) ;
#1609 = SHAPE_REPRESENTATION_RELATIONSHIP ( 'NONE' , 'NONE' ,  #2949, #2598 ) ;
#1610 = EDGE_CURVE ( 'NONE', #272, #973, #2433, .T. ) ;
#1611 = SHAPE_DEFINITION_REPRESENTATION ( #41, #961 ) ;
#1612 = FACE_OUTER_BOUND ( 'NONE', #3605, .T. ) ;
#1613 = CARTESIAN_POINT ( 'NONE',  ( 1.300000000000000044, -1.443375672974064328, 1.278502688459867223E-18 ) ) ;
#1614 = VERTEX_POINT ( 'NONE', #3061 ) ;
#1615 = FILL_AREA_STYLE ('',( #1578 ) ) ;
#1616 = ORIENTED_EDGE ( 'NONE', *, *, #804, .F. ) ;
#1617 = EDGE_CURVE ( 'NONE', #1003, #2788, #3746, .T. ) ;
#1618 = DIRECTION ( 'NONE',  ( -1.000000000000000000, -0.000000000000000000, -0.000000000000000000 ) ) ;
#1619 = APPLICATION_CONTEXT ( 'automotive_design' ) ;
#1620 = SPHERICAL_SURFACE ( 'NONE', #2881, 4.324969328314201000 ) ;
#1621 = ORIENTED_EDGE ( 'NONE', *, *, #2989, .T. ) ;
#1622 = DIRECTION ( 'NONE',  ( -0.7071067811865492381, 8.659560562354911904E-17, -0.7071067811865457964 ) ) ;
#1623 = CARTESIAN_POINT ( 'NONE',  ( 1.300000000000000044, -0.7216878364870318308, 1.249999999999999778 ) ) ;
#1624 = DIRECTION ( 'NONE',  ( -1.000000000000000000, -0.000000000000000000, -0.000000000000000000 ) ) ;
#1625 = CIRCLE ( 'NONE', #3802, 1.649999999999998579 ) ;
#1626 = EDGE_CURVE ( 'NONE', #1528, #691, #23, .T. ) ;
#1627 = PRESENTATION_LAYER_ASSIGNMENT (  '', '', ( #1564 ) ) ;
#1628 =( NAMED_UNIT ( * ) PLANE_ANGLE_UNIT ( ) SI_UNIT ( $, .RADIAN. ) );
#1629 = ORIENTED_EDGE ( 'NONE', *, *, #2634, .T. ) ;
#1630 = CARTESIAN_POINT ( 'NONE',  ( 2.200000000000000178, 0.000000000000000000, 0.000000000000000000 ) ) ;
#1631 = AXIS2_PLACEMENT_3D ( 'NONE', #1190, #2090, #2363 ) ;
#1632 = AXIS2_PLACEMENT_3D ( 'NONE', #496, #1689, #2869 ) ;
#1633 = AXIS2_PLACEMENT_3D ( 'NONE', #1289, #668, #77 ) ;
#1634 = AXIS2_PLACEMENT_3D ( 'NONE', #1354, #1558, #1891 ) ;
#1635 = CARTESIAN_POINT ( 'NONE',  ( 1.300000000000000044, -1.443375672974064328, 2.168404344971008868E-16 ) ) ;
#1636 = DIRECTION ( 'NONE',  ( -1.000000000000000000, -1.224646799147352961E-16, 0.000000000000000000 ) ) ;
#1637 = MECHANICAL_DESIGN_GEOMETRIC_PRESENTATION_REPRESENTATION (  '', ( #960 ), #1269 ) ;
#1638 = EDGE_CURVE ( 'NONE', #1107, #1166, #988, .T. ) ;
#1639 = VERTEX_POINT ( 'NONE', #1831 ) ;
#1640 = CARTESIAN_POINT ( 'NONE',  ( -89.85223847358115279, -17.40498196091244409, 5.000000000000000000 ) ) ;
#1641 = ORIENTED_EDGE ( 'NONE', *, *, #1820, .T. ) ;
#1642 = CYLINDRICAL_SURFACE ( 'NONE', #1950, 1.999999999999999112 ) ;
#1643 = UNCERTAINTY_MEASURE_WITH_UNIT (LENGTH_MEASURE( 1.000000000000000082E-05 ), #680, 'distance_accuracy_value', 'NONE');
#1644 = DIRECTION ( 'NONE',  ( -0.000000000000000000, -0.000000000000000000, -1.000000000000000000 ) ) ;
#1645 = EDGE_LOOP ( 'NONE', ( #3280, #1980, #1519, #2562, #408 ) ) ;
#1646 = CARTESIAN_POINT ( 'NONE',  ( 1.300000000000000044, 1.877893248421448789E-16, 1.250000000000000000 ) ) ;
#1647 = COLOUR_RGB ( '',1.000000000000000000, 0.9490196078431372140, 0.9098039215686274384 ) ;
#1648 = VECTOR ( 'NONE', #3079, 1000.000000000000000 ) ;
#1649 = CARTESIAN_POINT ( 'NONE',  ( 1.300000000000000044, 1.443375672974065216, 7.017607234860990640E-28 ) ) ;
#1650 = LINE ( 'NONE', #1314, #140 ) ;
#1651 = STYLED_ITEM ( 'NONE', ( #1453 ), #2870 ) ;
#1652 = AXIS2_PLACEMENT_3D ( 'NONE', #2785, #111, #2351 ) ;
#1653 = ORIENTED_EDGE ( 'NONE', *, *, #2499, .T. ) ;
#1654 = ORIENTED_EDGE ( 'NONE', *, *, #3224, .F. ) ;
#1655 = CARTESIAN_POINT ( 'NONE',  ( -3.749999999999998224, 29.76470224947664533, 5.000000000000000000 ) ) ;
#1656 = AXIS2_PLACEMENT_3D ( 'NONE', #3626, #1270, #3659 ) ;
#1657 = EDGE_CURVE ( 'NONE', #1614, #1542, #1315, .T. ) ;
#1658 = ORIENTED_EDGE ( 'NONE', *, *, #1758, .F. ) ;
#1659 = PRODUCT_CONTEXT ( 'NONE', #1175, 'mechanical' ) ;
#1660 = CARTESIAN_POINT ( 'NONE',  ( 0.000000000000000000, 0.000000000000000000, 5.000000000000000000 ) ) ;
#1661 = DIRECTION ( 'NONE',  ( -0.000000000000000000, -0.000000000000000000, -1.000000000000000000 ) ) ;
#1662 = CIRCLE ( 'NONE', #3545, 2.000000000000000000 ) ;
#1663 = ADVANCED_FACE ( 'NONE', ( #2470, #3656 ), #1534, .F. ) ;
#1664 = EDGE_LOOP ( 'NONE', ( #3316, #2404, #2850, #633 ) ) ;
#1665 = CARTESIAN_POINT ( 'NONE',  ( 0.000000000000000000, -1.443375672974064328, 1.278502688459867223E-18 ) ) ;
#1666 = ORIENTED_EDGE ( 'NONE', *, *, #3693, .T. ) ;
#1667 = ADVANCED_FACE ( 'NONE', ( #3289 ), #346, .F. ) ;
#1668 = DIRECTION ( 'NONE',  ( 0.000000000000000000, 0.000000000000000000, 1.000000000000000000 ) ) ;
#1669 = ADVANCED_FACE ( 'NONE', ( #2176 ), #1267, .T. ) ;
#1670 = DIRECTION ( 'NONE',  ( 0.000000000000000000, -0.8660254037844385966, 0.5000000000000001110 ) ) ;
#1671 = ORIENTED_EDGE ( 'NONE', *, *, #3077, .T. ) ;
#1672 = LINE ( 'NONE', #1124, #2834 ) ;
#1673 = DIRECTION ( 'NONE',  ( -1.000000000000000000, -0.000000000000000000, -0.000000000000000000 ) ) ;
#1674 = ORIENTED_EDGE ( 'NONE', *, *, #3782, .T. ) ;
#1675 = CARTESIAN_POINT ( 'NONE',  ( -70.00000000000000000, -21.41798680385620202, -30.00000000000000000 ) ) ;
#1676 = CARTESIAN_POINT ( 'NONE',  ( 2.200000000000000178, 0.000000000000000000, 0.000000000000000000 ) ) ;
#1677 = FILL_AREA_STYLE_COLOUR ( '', #847 ) ;
#1678 = SHAPE_DEFINITION_REPRESENTATION ( #3337, #2949 ) ;
#1679 = CARTESIAN_POINT ( 'NONE',  ( 0.000000000000000000, 0.7216878364870328300, 1.249999999999999778 ) ) ;
#1680 = CARTESIAN_POINT ( 'NONE',  ( 32.97619047619090793, 2.648642316818304643, 5.000000000000000000 ) ) ;
#1681 = ORIENTED_EDGE ( 'NONE', *, *, #3778, .F. ) ;
#1682 = PLANE ( 'NONE',  #1080 ) ;
#1683 = ORIENTED_EDGE ( 'NONE', *, *, #3565, .F. ) ;
#1684 = AXIS2_PLACEMENT_3D ( 'NONE', #3423, #2935, #3739 ) ;
#1685 = PRODUCT_DEFINITION_CONTEXT ( 'detailed design', #3101, 'design' ) ;
#1686 = CARTESIAN_POINT ( 'NONE',  ( 4.500000000000000000, 5.510910596163089556E-16, -24.00000000000000000 ) ) ;
#1687 = EDGE_LOOP ( 'NONE', ( #2677, #3663 ) ) ;
#1688 = CARTESIAN_POINT ( 'NONE',  ( 1.300000000000000044, 1.443375672974065216, 7.222237291452134449E-31 ) ) ;
#1689 = DIRECTION ( 'NONE',  ( -0.000000000000000000, -0.000000000000000000, -1.000000000000000000 ) ) ;
#1690 = EDGE_CURVE ( 'NONE', #2373, #715, #3622, .T. ) ;
#1691 = ORIENTED_EDGE ( 'NONE', *, *, #740, .F. ) ;
#1692 = CARTESIAN_POINT ( 'NONE',  ( -82.70833333333334281, -21.49672940239979724, 1.666666666666666297 ) ) ;
#1693 = FACE_OUTER_BOUND ( 'NONE', #2600, .T. ) ;
#1694 = FILL_AREA_STYLE ('',( #500 ) ) ;
#1695 = VECTOR ( 'NONE', #3815, 1000.000000000000000 ) ;
#1696 = DIRECTION ( 'NONE',  ( -1.000000000000000000, -0.000000000000000000, -0.000000000000000000 ) ) ;
#1697 = FILL_AREA_STYLE ('',( #1952 ) ) ;
#1698 = EDGE_CURVE ( 'NONE', #1729, #2556, #1551, .T. ) ;
#1699 = COLOUR_RGB ( '',1.000000000000000000, 0.9490196078431372140, 0.9098039215686274384 ) ;
#1700 = AXIS2_PLACEMENT_3D ( 'NONE', #3794, #3175, #1731 ) ;
#1701 = CIRCLE ( 'NONE', #2073, 1.249999999999999778 ) ;
#1702 = ORIENTED_EDGE ( 'NONE', *, *, #3508, .T. ) ;
#1703 =( NAMED_UNIT ( * ) PLANE_ANGLE_UNIT ( ) SI_UNIT ( $, .RADIAN. ) );
#1704 = ORIENTED_EDGE ( 'NONE', *, *, #1939, .F. ) ;
#1705 = PRODUCT_DEFINITION ( 'UNKNOWN', '', #1345, #794 ) ;
#1706 = VECTOR ( 'NONE', #1331, 999.9999999999998863 ) ;
#1707 = TOROIDAL_SURFACE ( 'NONE', #1197, 2.199999999999999289, 0.2000000000000000111 ) ;
#1708 = FACE_OUTER_BOUND ( 'NONE', #1485, .T. ) ;
#1709 = ORIENTED_EDGE ( 'NONE', *, *, #1339, .T. ) ;
#1710 = CARTESIAN_POINT ( 'NONE',  ( 0.000000000000000000, 0.000000000000000000, -30.00000000000000000 ) ) ;
#1711 = FACE_OUTER_BOUND ( 'NONE', #1380, .T. ) ;
#1712 = EDGE_CURVE ( 'NONE', #1151, #276, #3431, .T. ) ;
#1713 = AXIS2_PLACEMENT_3D ( 'NONE', #2356, #635, #3581 ) ;
#1714 = ORIENTED_EDGE ( 'NONE', *, *, #734, .T. ) ;
#1715 = CARTESIAN_POINT ( 'NONE',  ( 4.499999999999997335, 5.510910596163085611E-16, -30.00000000000000000 ) ) ;
#1716 = AXIS2_PLACEMENT_3D ( 'NONE', #2513, #381, #2144 ) ;
#1717 = VECTOR ( 'NONE', #2983, 1000.000000000000227 ) ;
#1718 = ORIENTED_EDGE ( 'NONE', *, *, #3186, .T. ) ;
#1719 = AXIS2_PLACEMENT_3D ( 'NONE', #2245, #2267, #1349 ) ;
#1720 = DIRECTION ( 'NONE',  ( 0.000000000000000000, 0.000000000000000000, 1.000000000000000000 ) ) ;
#1721 = DIRECTION ( 'NONE',  ( 1.000000000000000000, 0.000000000000000000, 0.000000000000000000 ) ) ;
#1722 = AXIS2_PLACEMENT_3D ( 'NONE', #316, #2846, #2645 ) ;
#1723 = ORIENTED_EDGE ( 'NONE', *, *, #3679, .T. ) ;
#1724 = ORIENTED_EDGE ( 'NONE', *, *, #3514, .T. ) ;
#1725 = B_SPLINE_CURVE_WITH_KNOTS ( 'NONE', 3,
 ( #505, #3456, #217, #1135, #3786, #1640 ),
 .UNSPECIFIED., .F., .F.,
 ( 4, 2, 4 ),
 ( 0.000000000000000000, 0.5000000000000000000, 1.000000000000000000 ),
 .UNSPECIFIED. ) ;
#1726 = ORIENTED_EDGE ( 'NONE', *, *, #2799, .F. ) ;
#1727 = DIRECTION ( 'NONE',  ( 0.000000000000000000, 0.000000000000000000, 1.000000000000000000 ) ) ;
#1728 = DIRECTION ( 'NONE',  ( 0.000000000000000000, 1.000000000000000000, -1.502314598737159031E-16 ) ) ;
#1729 = VERTEX_POINT ( 'NONE', #3349 ) ;
#1730 = CARTESIAN_POINT ( 'NONE',  ( 0.000000000000000000, 0.7216878364870329410, 1.249999999999999778 ) ) ;
#1731 = DIRECTION ( 'NONE',  ( 1.000000000000000000, 0.000000000000000000, 0.000000000000000000 ) ) ;
#1732 = ORIENTED_EDGE ( 'NONE', *, *, #3644, .F. ) ;
#1733 = ADVANCED_FACE ( 'NONE', ( #303, #1848 ), #679, .T. ) ;
#1734 = DIRECTION ( 'NONE',  ( -0.7071067811865492381, 0.000000000000000000, 0.7071067811865457964 ) ) ;
#1735 = SURFACE_SIDE_STYLE ('',( #3799 ) ) ;
#1736 = DIRECTION ( 'NONE',  ( -0.000000000000000000, -0.000000000000000000, -1.000000000000000000 ) ) ;
#1737 = VERTEX_POINT ( 'NONE', #3043 ) ;
#1738 = ORIENTED_EDGE ( 'NONE', *, *, #562, .F. ) ;
#1739 = CARTESIAN_POINT ( 'NONE',  ( 2.399999999999999911, 0.000000000000000000, 1.999999999999999112 ) ) ;
#1740 = VERTEX_POINT ( 'NONE', #923 ) ;
#1741 = CARTESIAN_POINT ( 'NONE',  ( 0.000000000000000000, 0.000000000000000000, -30.00000000000000000 ) ) ;
#1742 = APPLICATION_PROTOCOL_DEFINITION ( 'draft international standard', 'automotive_design', 1998, #3101 ) ;
#1743 = ORIENTED_EDGE ( 'NONE', *, *, #2063, .F. ) ;
#1744 = LINE ( 'NONE', #2916, #2484 ) ;
#1745 = CARTESIAN_POINT ( 'NONE',  ( -80.00000000000000000, 0.000000000000000000, -4.999999999999997335 ) ) ;
#1746 = ADVANCED_FACE ( 'NONE', ( #622 ), #3001, .T. ) ;
#1747 = ORIENTED_EDGE ( 'NONE', *, *, #1712, .T. ) ;
#1748 = DIRECTION ( 'NONE',  ( 0.000000000000000000, -0.4999999999999998890, 0.8660254037844387076 ) ) ;
#1749 = FACE_OUTER_BOUND ( 'NONE', #123, .T. ) ;
#1750 = SHAPE_REPRESENTATION_RELATIONSHIP ( 'NONE' , 'NONE' ,  #159, #791 ) ;
#1751 = SHAPE_REPRESENTATION ( 'o-rings series a_iso_O-ring 45x2.65-A-ISO 3601-1', ( #2207 ), #3327 ) ;
#1752 = AXIS2_PLACEMENT_3D ( 'NONE', #662, #2161, #699 ) ;
#1753 = CIRCLE ( 'NONE', #2192, 2.199999999999999289 ) ;
#1754 = CARTESIAN_POINT ( 'NONE',  ( 0.000000000000000000, 0.000000000000000000, 0.000000000000000000 ) ) ;
#1755 = VERTEX_POINT ( 'NONE', #780 ) ;
#1756 = AXIS2_PLACEMENT_3D ( 'NONE', #2851, #1083, #2557 ) ;
#1757 = CIRCLE ( 'NONE', #2264, 1.999999999999999112 ) ;
#1758 = EDGE_CURVE ( 'NONE', #3052, #1798, #3758, .T. ) ;
#1759 = EDGE_LOOP ( 'NONE', ( #2666, #2127 ) ) ;
#1760 =( NAMED_UNIT ( * ) SI_UNIT ( $, .STERADIAN. ) SOLID_ANGLE_UNIT ( ) );
#1761 = ORIENTED_EDGE ( 'NONE', *, *, #1827, .T. ) ;
#1762 = CARTESIAN_POINT ( 'NONE',  ( 18.99999999999999645, 2.326828918379970576E-15, -8.000000000000000000 ) ) ;
#1763 = AXIS2_PLACEMENT_3D ( 'NONE', #1276, #1004, #733 ) ;
#1764 = CARTESIAN_POINT ( 'NONE',  ( 30.00000000000000000, 0.000000000000000000, 0.000000000000000000 ) ) ;
#1765 = CIRCLE ( 'NONE', #2574, 1.649999999999998579 ) ;
#1766 = ITEM_DEFINED_TRANSFORMATION ( 'NONE', 'NONE', #1527,  #2207 ) ;
#1767 = ORIENTED_EDGE ( 'NONE', *, *, #546, .F. ) ;
#1768 = CARTESIAN_POINT ( 'NONE',  ( 1.300000000000000044, 1.082531754730548856, -0.6250000000000003331 ) ) ;
#1769 = CARTESIAN_POINT ( 'NONE',  ( 0.000000000000000000, 0.000000000000000000, -4.999999999999997335 ) ) ;
#1770 = DIRECTION ( 'NONE',  ( -0.9219985364506716463, 0.3871933609746164295, -2.048578313426146660E-17 ) ) ;
#1771 = VECTOR ( 'NONE', #2814, 1000.000000000000000 ) ;
#1772 = EDGE_LOOP ( 'NONE', ( #852, #1109 ) ) ;
#1773 = CARTESIAN_POINT ( 'NONE',  ( 0.000000000000000000, 1.443375672974065216, 7.222237291452134449E-31 ) ) ;
#1774 = CARTESIAN_POINT ( 'NONE',  ( 0.000000000000000000, 3.306546357697853733E-16, -2.700000000000000178 ) ) ;
#1775 = AXIS2_PLACEMENT_3D ( 'NONE', #1055, #2235, #3690 ) ;
#1776 = EDGE_CURVE ( 'NONE', #1889, #1255, #126, .T. ) ;
#1777 = EDGE_CURVE ( 'NONE', #328, #355, #1363, .T. ) ;
#1778 = VECTOR ( 'NONE', #1727, 1000.000000000000000 ) ;
#1779 = CARTESIAN_POINT ( 'NONE',  ( 2.200000000000000178, 0.000000000000000000, 3.799999999999999378 ) ) ;
#1780 = VERTEX_POINT ( 'NONE', #3158 ) ;
#1781 = VECTOR ( 'NONE', #1114, 1000.000000000000000 ) ;
#1782 = VERTEX_POINT ( 'NONE', #2487 ) ;
#1783 = EDGE_CURVE ( 'NONE', #1368, #3229, #1625, .T. ) ;
#1784 = VERTEX_POINT ( 'NONE', #3140 ) ;
#1785 = EDGE_CURVE ( 'NONE', #2036, #1148, #570, .T. ) ;
#1786 = CARTESIAN_POINT ( 'NONE',  ( 1.300000000000000044, -0.7216878364870318308, 1.249999999999999778 ) ) ;
#1787 = ORIENTED_EDGE ( 'NONE', *, *, #684, .F. ) ;
#1788 = DIRECTION ( 'NONE',  ( -1.000000000000000000, 0.000000000000000000, 0.000000000000000000 ) ) ;
#1789 = SURFACE_SIDE_STYLE ('',( #315 ) ) ;
#1790 = ORIENTED_EDGE ( 'NONE', *, *, #3606, .T. ) ;
#1791 = DIRECTION ( 'NONE',  ( 0.000000000000000000, 0.000000000000000000, 1.000000000000000000 ) ) ;
#1792 = CARTESIAN_POINT ( 'NONE',  ( 0.000000000000000000, 0.000000000000000000, 0.000000000000000000 ) ) ;
#1793 =( NAMED_UNIT ( * ) PLANE_ANGLE_UNIT ( ) SI_UNIT ( $, .RADIAN. ) );
#1794 = PRODUCT_DEFINITION ( 'UNKNOWN', '', #853, #2727 ) ;
#1795 = PRODUCT ( 'socket button head screw_iso_ISO 7380 - M4 x 10 - 10N', 'socket button head screw_iso_ISO 7380 - M4 x 10 - 10N', '', ( #1347 ) ) ;
#1796 = FACE_OUTER_BOUND ( 'NONE', #1664, .T. ) ;
#1797 = ORIENTED_EDGE ( 'NONE', *, *, #461, .F. ) ;
#1798 = VERTEX_POINT ( 'NONE', #1655 ) ;
#1799 = VERTEX_POINT ( 'NONE', #1909 ) ;
#1800 = PLANE ( 'NONE',  #1268 ) ;
#1801 = EDGE_LOOP ( 'NONE', ( #1174, #1412, #223, #3437 ) ) ;
#1802 = CARTESIAN_POINT ( 'NONE',  ( 2.399999999999999911, 2.449293598294705428E-16, -1.999999999999999112 ) ) ;
#1803 = DIRECTION ( 'NONE',  ( 1.000000000000000000, 0.000000000000000000, 0.000000000000000000 ) ) ;
#1804 = FACE_OUTER_BOUND ( 'NONE', #1120, .T. ) ;
#1805 = DIRECTION ( 'NONE',  ( -1.241531209392323001E-18, -5.843967824224479992E-17, 1.000000000000000000 ) ) ;
#1806 = ADVANCED_FACE ( 'NONE', ( #2261 ), #188, .T. ) ;
#1807 = ORIENTED_EDGE ( 'NONE', *, *, #3083, .T. ) ;
#1808 = CARTESIAN_POINT ( 'NONE',  ( -82.50000000000000000, -19.84313483298442904, -4.999999999999997335 ) ) ;
#1809 = CARTESIAN_POINT ( 'NONE',  ( 30.00000000000000000, 0.000000000000000000, 0.000000000000000000 ) ) ;
#1810 =( NAMED_UNIT ( * ) SI_UNIT ( $, .STERADIAN. ) SOLID_ANGLE_UNIT ( ) );
#1811 = EDGE_CURVE ( 'NONE', #2788, #1003, #887, .T. ) ;
#1812 = CARTESIAN_POINT ( 'NONE',  ( 0.000000000000000000, 0.000000000000000000, 0.000000000000000000 ) ) ;
#1813 = VERTEX_POINT ( 'NONE', #1096 ) ;
#1814 = AXIS2_PLACEMENT_3D ( 'NONE', #1792, #2593, #2923 ) ;
#1815 = ORIENTED_EDGE ( 'NONE', *, *, #3449, .F. ) ;
#1816 = ORIENTED_EDGE ( 'NONE', *, *, #3736, .F. ) ;
#1817 = CARTESIAN_POINT ( 'NONE',  ( 3.885274725274726393, -8.673617379884035472E-16, 0.000000000000000000 ) ) ;
#1818=STYLED_ITEM('',(#3881),#3290);
#1819 = ADVANCED_FACE ( 'NONE', ( #2288 ), #948, .T. ) ;
#1820 = EDGE_CURVE ( 'NONE', #1151, #3666, #3673, .T. ) ;
#1821 = APPLICATION_CONTEXT ( 'automotive_design' ) ;
#1822 = AXIS2_PLACEMENT_3D ( 'NONE', #1306, #3627, #3351 ) ;
#1823 = AXIS2_PLACEMENT_3D ( 'NONE', #1428, #3237, #1125 ) ;
#1824 = VERTEX_POINT ( 'NONE', #3104 ) ;
#1825 = PLANE ( 'NONE',  #1023 ) ;
#1826 = FACE_OUTER_BOUND ( 'NONE', #161, .T. ) ;
#1827 = EDGE_CURVE ( 'NONE', #511, #673, #124, .T. ) ;
#1828 = VECTOR ( 'NONE', #2387, 999.9999999999998863 ) ;
#1829 = UNCERTAINTY_MEASURE_WITH_UNIT (LENGTH_MEASURE( 1.000000000000000082E-05 ), #1383, 'distance_accuracy_value', 'NONE');
#1830 = LINE ( 'NONE', #586, #3698 ) ;
#1831 = CARTESIAN_POINT ( 'NONE',  ( 0.000000000000000000, 0.000000000000000000, 2.700000000000000178 ) ) ;
#1832 = SHAPE_REPRESENTATION_RELATIONSHIP ( 'NONE' , 'NONE' ,  #1751, #2924 ) ;
#1833 = EDGE_CURVE ( 'NONE', #2247, #3559, #3372, .T. ) ;
#1834 = LINE ( 'NONE', #94, #726 ) ;
#1835 = DIRECTION ( 'NONE',  ( -1.224646799147353207E-16, 1.000000000000000000, 0.000000000000000000 ) ) ;
#1836 =( GEOMETRIC_REPRESENTATION_CONTEXT ( 3 ) GLOBAL_UNCERTAINTY_ASSIGNED_CONTEXT ( ( #3509 ) ) GLOBAL_UNIT_ASSIGNED_CONTEXT ( ( #3759, #2289, #2508 ) ) REPRESENTATION_CONTEXT ( 'NONE', 'WORKASPACE' ) );
#1837 = ORIENTED_EDGE ( 'NONE', *, *, #3556, .F. ) ;
#1838 = FILL_AREA_STYLE ('',( #3608 ) ) ;
#1839 = ORIENTED_EDGE ( 'NONE', *, *, #1896, .F. ) ;
#1840 = CIRCLE ( 'NONE', #341, 3.799999999999999378 ) ;
#1841 = DIRECTION ( 'NONE',  ( -1.000000000000000000, 0.000000000000000000, 0.000000000000000000 ) ) ;
#1842 = ORIENTED_EDGE ( 'NONE', *, *, #2292, .T. ) ;
#1843 = CARTESIAN_POINT ( 'NONE',  ( 0.000000000000000000, 0.000000000000000000, 3.799999999999999378 ) ) ;
#1844 = FACE_BOUND ( 'NONE', #3433, .T. ) ;
#1845 = CARTESIAN_POINT ( 'NONE',  ( 0.000000000000000000, 0.000000000000000000, -20.00000000000000000 ) ) ;
#1846 = ADVANCED_FACE ( 'NONE', ( #1319 ), #2378, .F. ) ;
#1847 = DIRECTION ( 'NONE',  ( 0.000000000000000000, 0.000000000000000000, 1.000000000000000000 ) ) ;
#1848 = FACE_BOUND ( 'NONE', #3445, .T. ) ;
#1849 = EDGE_CURVE ( 'NONE', #3489, #926, #763, .T. ) ;
#1850 = CARTESIAN_POINT ( 'NONE',  ( -82.50000000000000000, -19.84313483298442904, -30.00000000000000000 ) ) ;
#1851 = CARTESIAN_POINT ( 'NONE',  ( -80.00000000000000000, 0.000000000000000000, 0.001000000000000132727 ) ) ;
#1852 = ORIENTED_EDGE ( 'NONE', *, *, #1133, .T. ) ;
#1853 = LINE ( 'NONE', #474, #639 ) ;
#1854 = ORIENTED_EDGE ( 'NONE', *, *, #2283, .F. ) ;
#1855 = DIRECTION ( 'NONE',  ( -1.000000000000000000, 0.000000000000000000, 0.000000000000000000 ) ) ;
#1856 = FACE_OUTER_BOUND ( 'NONE', #453, .T. ) ;
#1857 = ORIENTED_EDGE ( 'NONE', *, *, #482, .T. ) ;
#1858 = LINE ( 'NONE', #2528, #3702 ) ;
#1859 = ADVANCED_FACE ( 'NONE', ( #2221 ), #3407, .F. ) ;
#1860 = CARTESIAN_POINT ( 'NONE',  ( -3.750000000000001776, -29.76470224947664178, -30.00000000000000000 ) ) ;
#1861 = CARTESIAN_POINT ( 'NONE',  ( 8.673617379884035472E-16, -1.899999999999999689, -3.490243377569955075E-16 ) ) ;
#1862 = FILL_AREA_STYLE ('',( #3657 ) ) ;
#1863 = ADVANCED_FACE ( 'NONE', ( #149 ), #759, .T. ) ;
#1864 = FACE_OUTER_BOUND ( 'NONE', #293, .T. ) ;
#1865 = DIRECTION ( 'NONE',  ( 0.000000000000000000, -0.8660254037844385966, -0.5000000000000001110 ) ) ;
#1866 = ADVANCED_FACE ( 'NONE', ( #1060 ), #1417, .T. ) ;
#1867 = ORIENTED_EDGE ( 'NONE', *, *, #2070, .T. ) ;
#1868 = DIRECTION ( 'NONE',  ( 1.000000000000000000, 0.000000000000000000, -0.000000000000000000 ) ) ;
#1869 = EDGE_LOOP ( 'NONE', ( #2204, #2702, #2155, #2272 ) ) ;
#1870 = CARTESIAN_POINT ( 'NONE',  ( 0.000000000000000000, 0.000000000000000000, -20.00000000000000000 ) ) ;
#1871 = CIRCLE ( 'NONE', #3064, 4.324969328314200112 ) ;
#1872 = CYLINDRICAL_SURFACE ( 'NONE', #2700, 4.499999999999997335 ) ;
#1873 = VERTEX_POINT ( 'NONE', #1168 ) ;
#1874 = DIRECTION ( 'NONE',  ( 0.000000000000000000, 0.000000000000000000, 1.000000000000000000 ) ) ;
#1875 = AXIS2_PLACEMENT_3D ( 'NONE', #1997, #534, #1425 ) ;
#1876 = DIRECTION ( 'NONE',  ( -1.000000000000000000, -0.000000000000000000, -0.000000000000000000 ) ) ;
#1877 = DIRECTION ( 'NONE',  ( 0.000000000000000000, 0.000000000000000000, 1.000000000000000000 ) ) ;
#1878=STYLED_ITEM('',(#3888),#3238);
#1879 = VECTOR ( 'NONE', #515, 1000.000000000000000 ) ;
#1880 = DIRECTION ( 'NONE',  ( 0.000000000000000000, 0.000000000000000000, 1.000000000000000000 ) ) ;
#1881 = ORIENTED_EDGE ( 'NONE', *, *, #2153, .T. ) ;
#1882 = CARTESIAN_POINT ( 'NONE',  ( -3.750000000000004441, 29.76470224947664533, -30.00000000000000000 ) ) ;
#1883 = CIRCLE ( 'NONE', #645, 5.000000000000004441 ) ;
#1884 = VECTOR ( 'NONE', #2349, 1000.000000000000000 ) ;
#1885 = DIRECTION ( 'NONE',  ( -1.000000000000000000, 0.000000000000000000, 0.000000000000000000 ) ) ;
#1886 = DIRECTION ( 'NONE',  ( -1.000000000000000000, 0.000000000000000000, 0.000000000000000000 ) ) ;
#1887 = ADVANCED_FACE ( 'NONE', ( #2047 ), #2605, .F. ) ;
#1888 = AXIS2_PLACEMENT_3D ( 'NONE', #120, #357, #1920 ) ;
#1889 = VERTEX_POINT ( 'NONE', #560 ) ;
#1890 = ORIENTED_EDGE ( 'NONE', *, *, #2965, .T. ) ;
#1891 = DIRECTION ( 'NONE',  ( 0.9921567416492214075, 0.1250000000000001388, 0.000000000000000000 ) ) ;
#1892 = APPLICATION_CONTEXT ( 'automotive_design' ) ;
#1893 = EDGE_CURVE ( 'NONE', #2934, #355, #3558, .T. ) ;
#1894 = COLOUR_RGB ( '',0.8941176470588234615, 0.8941176470588234615, 0.8941176470588234615 ) ;
#1895 = VECTOR ( 'NONE', #3405, 1000.000000000000000 ) ;
#1896 = EDGE_CURVE ( 'NONE', #748, #3752, #1198, .T. ) ;
#1897 = EDGE_CURVE ( 'NONE', #757, #2595, #377, .T. ) ;
#1898 =( GEOMETRIC_REPRESENTATION_CONTEXT ( 3 ) GLOBAL_UNCERTAINTY_ASSIGNED_CONTEXT ( ( #1996 ) ) GLOBAL_UNIT_ASSIGNED_CONTEXT ( ( #2450, #2177, #376 ) ) REPRESENTATION_CONTEXT ( 'NONE', 'WORKASPACE' ) );
#1899 = AXIS2_PLACEMENT_3D ( 'NONE', #1467, #2662, #2417 ) ;
#1900 = CARTESIAN_POINT ( 'NONE',  ( -75.00000000000000000, 0.000000000000000000, -5.000000000000000000 ) ) ;
#1901 = ORIENTED_EDGE ( 'NONE', *, *, #106, .F. ) ;
#1902 = CARTESIAN_POINT ( 'NONE',  ( -3.749999999999998224, 29.76470224947664533, -30.00000000000000000 ) ) ;
#1903 = DIRECTION ( 'NONE',  ( -0.000000000000000000, 0.000000000000000000, 1.000000000000000000 ) ) ;
#1904 = FACE_OUTER_BOUND ( 'NONE', #2436, .T. ) ;
#1905 = CIRCLE ( 'NONE', #3773, 2.000000000000000000 ) ;
#1906 = PRODUCT ( 'specimen holder', 'specimen holder', '', ( #784 ) ) ;
#1907 = LINE ( 'NONE', #1902, #2711 ) ;
#1908 = ORIENTED_EDGE ( 'NONE', *, *, #3326, .T. ) ;
#1909 = CARTESIAN_POINT ( 'NONE',  ( -90.00000000000000000, 0.000000000000000000, -4.999999999999997335 ) ) ;
#1910 = PLANE ( 'NONE',  #2257 ) ;
#1911 = DIRECTION ( 'NONE',  ( -1.000000000000000000, -0.000000000000000000, -0.000000000000000000 ) ) ;
#1912 = ORIENTED_EDGE ( 'NONE', *, *, #1133, .F. ) ;
#1913 =( NAMED_UNIT ( * ) PLANE_ANGLE_UNIT ( ) SI_UNIT ( $, .RADIAN. ) );
#1914 = ORIENTED_EDGE ( 'NONE', *, *, #567, .T. ) ;
#1915 = DIRECTION ( 'NONE',  ( -1.000000000000000000, 0.000000000000000000, 0.000000000000000000 ) ) ;
#1916 = UNCERTAINTY_MEASURE_WITH_UNIT (LENGTH_MEASURE( 1.000000000000000082E-05 ), #2623, 'distance_accuracy_value', 'NONE');
#1917 = DIRECTION ( 'NONE',  ( 0.000000000000000000, 0.000000000000000000, 1.000000000000000000 ) ) ;
#1918 = ORIENTED_EDGE ( 'NONE', *, *, #707, .F. ) ;
#1919 = CARTESIAN_POINT ( 'NONE',  ( 0.000000000000000000, -0.7216878364870317197, -1.250000000000000000 ) ) ;
#1920 = DIRECTION ( 'NONE',  ( 0.000000000000000000, 0.000000000000000000, 1.000000000000000000 ) ) ;
#1921 = DIRECTION ( 'NONE',  ( 0.000000000000000000, 0.000000000000000000, 1.000000000000000000 ) ) ;
#1922 = CARTESIAN_POINT ( 'NONE',  ( 34.99999999999999289, 0.000000000000000000, -30.00000000000000000 ) ) ;
#1923 = ORIENTED_EDGE ( 'NONE', *, *, #1100, .T. ) ;
#1924 = DIRECTION ( 'NONE',  ( -0.000000000000000000, -0.000000000000000000, -1.000000000000000000 ) ) ;
#1925 = ADVANCED_FACE ( 'NONE', ( #3189 ), #1134, .F. ) ;
#1926 = SHAPE_DEFINITION_REPRESENTATION ( #3429, #159 ) ;
#1927 = CARTESIAN_POINT ( 'NONE',  ( 1.300000000000000044, 0.7216878364870329410, 1.249999999999999778 ) ) ;
#1928 =( NAMED_UNIT ( * ) SI_UNIT ( $, .STERADIAN. ) SOLID_ANGLE_UNIT ( ) );
#1929 = ADVANCED_FACE ( 'NONE', ( #1693 ), #74, .F. ) ;
#1930 = ORIENTED_EDGE ( 'NONE', *, *, #1970, .T. ) ;
#1931 = ORIENTED_EDGE ( 'NONE', *, *, #3166, .T. ) ;
#1932 = DIRECTION ( 'NONE',  ( -1.000000000000000000, -0.000000000000000000, -0.000000000000000000 ) ) ;
#1933 = CARTESIAN_POINT ( 'NONE',  ( -2.899999999999999911, 0.000000000000000000, 0.000000000000000000 ) ) ;
#1934 = ORIENTED_EDGE ( 'NONE', *, *, #2178, .T. ) ;
#1935 = DIRECTION ( 'NONE',  ( 0.000000000000000000, 0.000000000000000000, 1.000000000000000000 ) ) ;
#1936 = DIRECTION ( 'NONE',  ( -1.000000000000000000, -0.000000000000000000, -0.000000000000000000 ) ) ;
#1937 = CARTESIAN_POINT ( 'NONE',  ( -82.50000000000000000, -19.84313483298442904, 0.000000000000000000 ) ) ;
#1938 = AXIS2_PLACEMENT_3D ( 'NONE', #3176, #2573, #1020 ) ;
#1939 = EDGE_CURVE ( 'NONE', #2587, #3455, #288, .T. ) ;
#1940 = MECHANICAL_DESIGN_GEOMETRIC_PRESENTATION_REPRESENTATION (  '', ( #1564 ), #576 ) ;
#1941 = ORIENTED_EDGE ( 'NONE', *, *, #2637, .F. ) ;
#1942 = ORIENTED_EDGE ( 'NONE', *, *, #2920, .F. ) ;
#1943 = CARTESIAN_POINT ( 'NONE',  ( 3.885274725274726393, -8.673617379884035472E-16, 0.000000000000000000 ) ) ;
#1944 = ADVANCED_FACE ( 'NONE', ( #286 ), #2669, .T. ) ;
#1945=STYLED_ITEM('',(#3881),#3253);
#1946 = VECTOR ( 'NONE', #1483, 1000.000000000000000 ) ;
#1947 = EDGE_CURVE ( 'NONE', #1374, #1577, #2321, .T. ) ;
#1948 = PRODUCT_CONTEXT ( 'NONE', #2027, 'mechanical' ) ;
#1949 = EDGE_CURVE ( 'NONE', #2595, #757, #3246, .T. ) ;
#1950 = AXIS2_PLACEMENT_3D ( 'NONE', #3396, #1618, #1065 ) ;
#1951 = DIRECTION ( 'NONE',  ( 0.000000000000000000, 0.000000000000000000, 1.000000000000000000 ) ) ;
#1952 = FILL_AREA_STYLE_COLOUR ( '', #2956 ) ;
#1953 = AXIS2_PLACEMENT_3D ( 'NONE', #2599, #182, #2298 ) ;
#1954 = VERTEX_POINT ( 'NONE', #2936 ) ;
#1955 = DIRECTION ( 'NONE',  ( 1.000000000000000000, 0.000000000000000000, 0.000000000000000000 ) ) ;
#1956 = ORIENTED_EDGE ( 'NONE', *, *, #2275, .T. ) ;
#1957 = LINE ( 'NONE', #476, #2077 ) ;
#1958 = UNCERTAINTY_MEASURE_WITH_UNIT (LENGTH_MEASURE( 1.000000000000000082E-05 ), #3266, 'distance_accuracy_value', 'NONE');
#1959 = CARTESIAN_POINT ( 'NONE',  ( 0.000000000000000000, 0.000000000000000000, -14.99999999999999645 ) ) ;
#1960 = ORIENTED_EDGE ( 'NONE', *, *, #1712, .F. ) ;
#1961 = DIRECTION ( 'NONE',  ( 0.000000000000000000, 0.000000000000000000, 1.000000000000000000 ) ) ;
#1962 = CIRCLE ( 'NONE', #1716, 30.00000000000000000 ) ;
#1963 = AXIS2_PLACEMENT_3D ( 'NONE', #3021, #1510, #2708 ) ;
#1964 = DIRECTION ( 'NONE',  ( 1.000000000000000000, 0.000000000000000000, 0.000000000000000000 ) ) ;
#1965 = AXIS2_PLACEMENT_3D ( 'NONE', #2563, #495, #3475 ) ;
#1966 = MANIFOLD_SOLID_BREP ( 'CBORE for M4 Pan Head Screw1', #3341 ) ;
#1967 = ORIENTED_EDGE ( 'NONE', *, *, #3796, .F. ) ;
#1968 = CARTESIAN_POINT ( 'NONE',  ( 8.673617379884035472E-16, 0.000000000000000000, 0.000000000000000000 ) ) ;
#1969 = DIRECTION ( 'NONE',  ( 0.000000000000000000, 0.000000000000000000, 1.000000000000000000 ) ) ;
#1970 = EDGE_CURVE ( 'NONE', #605, #3181, #1753, .T. ) ;
#1971 = CIRCLE ( 'NONE', #2150, 3.799999999999999378 ) ;
#1972 = APPLICATION_PROTOCOL_DEFINITION ( 'draft international standard', 'automotive_design', 1998, #626 ) ;
#1973 = LINE ( 'NONE', #420, #158 ) ;
#1974 = PRESENTATION_STYLE_ASSIGNMENT (( #2268 ) ) ;
#1975 = PRODUCT_DEFINITION_SHAPE ( 'NONE', 'NONE',  #3576 ) ;
#1976 = ORIENTED_EDGE ( 'NONE', *, *, #3737, .F. ) ;
#1977 = DIRECTION ( 'NONE',  ( 1.000000000000000000, 0.000000000000000000, 0.000000000000000000 ) ) ;
#1978 = EDGE_LOOP ( 'NONE', ( #3148, #2950, #2603 ) ) ;
#1979 = CARTESIAN_POINT ( 'NONE',  ( 2.000000000000001776, 2.449293598294708880E-16, -20.00000000000000000 ) ) ;
#1980 = ORIENTED_EDGE ( 'NONE', *, *, #417, .T. ) ;
#1981 = DIRECTION ( 'NONE',  ( -0.9921567416492214075, 0.1250000000000000555, 0.000000000000000000 ) ) ;
#1982 = CARTESIAN_POINT ( 'NONE',  ( 33.33333333333333570, 0.000000000000000000, 3.333333333333331705 ) ) ;
#1983 = EDGE_CURVE ( 'NONE', #1755, #3052, #658, .T. ) ;
#1984 = EDGE_LOOP ( 'NONE', ( #1063, #1918, #1691, #1852 ) ) ;
#1985 = CARTESIAN_POINT ( 'NONE',  ( 1.649999999999999911, 0.000000000000000000, -15.70000000000000284 ) ) ;
#1986 = DIRECTION ( 'NONE',  ( 0.000000000000000000, 0.000000000000000000, -1.000000000000000000 ) ) ;
#1987 = UNCERTAINTY_MEASURE_WITH_UNIT (LENGTH_MEASURE( 1.000000000000000082E-05 ), #3301, 'distance_accuracy_value', 'NONE');
#1988 = ADVANCED_FACE ( 'NONE', ( #1804 ), #2996, .F. ) ;
#1989 = DIRECTION ( 'NONE',  ( -1.000000000000000000, -0.000000000000000000, -0.000000000000000000 ) ) ;
#1990 = SURFACE_STYLE_FILL_AREA ( #1697 ) ;
#1991 = EDGE_LOOP ( 'NONE', ( #160, #1361, #1561, #2928 ) ) ;
#1992 = CARTESIAN_POINT ( 'NONE',  ( -90.00000000000000000, -17.32050807568877460, -30.00000000000000000 ) ) ;
#1993 = ORIENTED_EDGE ( 'NONE', *, *, #3765, .F. ) ;
#1994 = ADVANCED_FACE ( 'NONE', ( #3635 ), #3325, .F. ) ;
#1995 = MANIFOLD_SOLID_BREP ( 'Hex', #2346 ) ;
#1996 = UNCERTAINTY_MEASURE_WITH_UNIT (LENGTH_MEASURE( 1.000000000000000082E-05 ), #2450, 'distance_accuracy_value', 'NONE');
#1997 = CARTESIAN_POINT ( 'NONE',  ( 34.99999999999999289, 0.000000000000000000, 5.000000000000000000 ) ) ;
#1998 = ORIENTED_EDGE ( 'NONE', *, *, #231, .F. ) ;
#1999 = CARTESIAN_POINT ( 'NONE',  ( 30.00000000000000000, 0.000000000000000000, 0.000000000000000000 ) ) ;
#2000 = DIRECTION ( 'NONE',  ( -1.000000000000000000, -0.000000000000000000, -0.000000000000000000 ) ) ;
#2001 = VERTEX_POINT ( 'NONE', #2685 ) ;
#2002 = DIRECTION ( 'NONE',  ( -0.000000000000000000, -0.000000000000000000, -1.000000000000000000 ) ) ;
#2003 =( LENGTH_UNIT ( ) NAMED_UNIT ( * ) SI_UNIT ( .MILLI., .METRE. ) );
#2004 = VECTOR ( 'NONE', #3364, 1000.000000000000000 ) ;
#2005 = ORIENTED_EDGE ( 'NONE', *, *, #3049, .F. ) ;
#2006 = CARTESIAN_POINT ( 'NONE',  ( 1.600000000000000089, 0.000000000000000000, 0.000000000000000000 ) ) ;
#2007 = CARTESIAN_POINT ( 'NONE',  ( 0.000000000000000000, 0.000000000000000000, -20.00000000000000000 ) ) ;
#2008 = VECTOR ( 'NONE', #3163, 1000.000000000000000 ) ;
#2009 = VECTOR ( 'NONE', #2136, 1000.000000000000000 ) ;
#2010 = AXIS2_PLACEMENT_3D ( 'NONE', #3818, #1156, #2344 ) ;
#2011 = VECTOR ( 'NONE', #3361, 1000.000000000000000 ) ;
#2012 = VERTEX_POINT ( 'NONE', #3554 ) ;
#2013 = ORIENTED_EDGE ( 'NONE', *, *, #1571, .T. ) ;
#2014 = CIRCLE ( 'NONE', #2761, 5.000000000000004441 ) ;
#2015 = DIRECTION ( 'NONE',  ( -0.000000000000000000, -0.000000000000000000, -1.000000000000000000 ) ) ;
#2016 = ORIENTED_EDGE ( 'NONE', *, *, #3679, .F. ) ;
#2017 = LINE ( 'NONE', #2893, #1778 ) ;
#2018 = CARTESIAN_POINT ( 'NONE',  ( 0.000000000000000000, 0.000000000000000000, -20.00000000000000000 ) ) ;
#2019 = EDGE_CURVE ( 'NONE', #3147, #1255, #1263, .T. ) ;
#2020 = CIRCLE ( 'NONE', #2515, 1.250000000000000222 ) ;
#2021 = MANIFOLD_SOLID_BREP ( 'AdvancedHole1', #2664 ) ;
#2022 = VECTOR ( 'NONE', #1538, 1000.000000000000000 ) ;
#2023 = ORIENTED_EDGE ( 'NONE', *, *, #368, .F. ) ;
#2024 = DIRECTION ( 'NONE',  ( 1.000000000000000000, 0.000000000000000000, 0.000000000000000000 ) ) ;
#2025 =( NAMED_UNIT ( * ) PLANE_ANGLE_UNIT ( ) SI_UNIT ( $, .RADIAN. ) );
#2026 = DIRECTION ( 'NONE',  ( 1.795453617517838962E-17, -1.015442787603507307E-17, -1.000000000000000222 ) ) ;
#2027 = APPLICATION_CONTEXT ( 'automotive_design' ) ;
#2028 = CIRCLE ( 'NONE', #150, 3.799999999999999378 ) ;
#2029 = CIRCLE ( 'NONE', #334, 3.799999999999999378 ) ;
#2030 = EDGE_LOOP ( 'NONE', ( #1142, #790, #2438 ) ) ;
#2031 = VECTOR ( 'NONE', #175, 999.9999999999998863 ) ;
#2032 = CARTESIAN_POINT ( 'NONE',  ( 1.300000000000000044, 0.000000000000000000, -1.250000000000000000 ) ) ;
#2033 = EDGE_CURVE ( 'NONE', #1187, #1528, #2394, .T. ) ;
#2034 = PRODUCT_DEFINITION_FORMATION_WITH_SPECIFIED_SOURCE ( 'ANY', '', #1795, .NOT_KNOWN. ) ;
#2035 = FACE_OUTER_BOUND ( 'NONE', #1024, .T. ) ;
#2036 = VERTEX_POINT ( 'NONE', #57 ) ;
#2037 = UNCERTAINTY_MEASURE_WITH_UNIT (LENGTH_MEASURE( 1.000000000000000082E-05 ), #3534, 'distance_accuracy_value', 'NONE');
#2038 = VERTEX_POINT ( 'NONE', #3618 ) ;
#2039 = DIRECTION ( 'NONE',  ( -1.000000000000000000, -0.000000000000000000, -0.000000000000000000 ) ) ;
#2040 = ORIENTED_EDGE ( 'NONE', *, *, #3678, .F. ) ;
#2041 = DIRECTION ( 'NONE',  ( 0.000000000000000000, 0.000000000000000000, 1.000000000000000000 ) ) ;
#2042 = ADVANCED_FACE ( 'NONE', ( #756 ), #121, .T. ) ;
#2043 = DIRECTION ( 'NONE',  ( 1.000000000000000000, 0.000000000000000000, 0.000000000000000000 ) ) ;
#2044 = APPLICATION_PROTOCOL_DEFINITION ( 'draft international standard', 'automotive_design', 1998, #1421 ) ;
#2045 = ORIENTED_EDGE ( 'NONE', *, *, #684, .T. ) ;
#2046 = DIRECTION ( 'NONE',  ( -0.000000000000000000, -0.5000000000000001110, 0.8660254037844385966 ) ) ;
#2047 = FACE_OUTER_BOUND ( 'NONE', #3318, .T. ) ;
#2048 = ORIENTED_EDGE ( 'NONE', *, *, #2747, .T. ) ;
#2049 = DIRECTION ( 'NONE',  ( -0.000000000000000000, 1.000000000000000000, -0.000000000000000000 ) ) ;
#2050 = EDGE_CURVE ( 'NONE', #3752, #201, #695, .T. ) ;
#2051 = CARTESIAN_POINT ( 'NONE',  ( 0.000000000000000000, 0.7216878364870328300, -1.250000000000000000 ) ) ;
#2052 = ORIENTED_EDGE ( 'NONE', *, *, #46, .T. ) ;
#2053 = EDGE_LOOP ( 'NONE', ( #1709, #1409, #1718, #295, #2907 ) ) ;
#2054 = PRESENTATION_STYLE_ASSIGNMENT (( #3529 ) ) ;
#2055 = ORIENTED_EDGE ( 'NONE', *, *, #1274, .F. ) ;
#2056 = DIRECTION ( 'NONE',  ( -0.000000000000000000, 0.000000000000000000, 1.000000000000000000 ) ) ;
#2057 = DIRECTION ( 'NONE',  ( 1.000000000000000000, 0.000000000000000000, 0.000000000000000000 ) ) ;
#2058 = CONTEXT_DEPENDENT_SHAPE_REPRESENTATION ( #3216, #2218 ) ;
#2059 = EDGE_LOOP ( 'NONE', ( #2408, #183, #3661, #1415 ) ) ;
#2060 = FACE_OUTER_BOUND ( 'NONE', #2676, .T. ) ;
#2061 = DIRECTION ( 'NONE',  ( -0.000000000000000000, -0.000000000000000000, -1.000000000000000000 ) ) ;
#2062 = CARTESIAN_POINT ( 'NONE',  ( 0.000000000000000000, 0.000000000000000000, 0.000000000000000000 ) ) ;
#2063 = EDGE_CURVE ( 'NONE', #3050, #143, #3100, .T. ) ;
#2064 = EDGE_CURVE ( 'NONE', #3822, #80, #2382, .T. ) ;
#2065 = ORIENTED_EDGE ( 'NONE', *, *, #1983, .T. ) ;
#2066 = DIRECTION ( 'NONE',  ( -1.000000000000000000, -0.000000000000000000, -0.000000000000000000 ) ) ;
#2067 = DIRECTION ( 'NONE',  ( 1.000000000000000000, 0.000000000000000000, 0.000000000000000000 ) ) ;
#2068 = VECTOR ( 'NONE', #44, 1000.000000000000114 ) ;
#2069 = ADVANCED_FACE ( 'NONE', ( #1904 ), #718, .T. ) ;
#2070 = EDGE_CURVE ( 'NONE', #1408, #1, #1139, .T. ) ;
#2071 = DIRECTION ( 'NONE',  ( -0.000000000000000000, 0.000000000000000000, 1.000000000000000000 ) ) ;
#2072 = VERTEX_POINT ( 'NONE', #3135 ) ;
#2073 = AXIS2_PLACEMENT_3D ( 'NONE', #1146, #2617, #2315 ) ;
#2074 = ORIENTED_EDGE ( 'NONE', *, *, #905, .F. ) ;
#2075 = DIRECTION ( 'NONE',  ( 0.000000000000000000, -1.000000000000000000, 0.000000000000000000 ) ) ;
#2076 = EDGE_LOOP ( 'NONE', ( #2425, #3757, #3548, #946 ) ) ;
#2077 = VECTOR ( 'NONE', #3749, 1000.000000000000000 ) ;
#2078 = CARTESIAN_POINT ( 'NONE',  ( 2.000000000000000000, 2.449293598294706414E-16, -15.70000000000000284 ) ) ;
#2079 = ORIENTED_EDGE ( 'NONE', *, *, #3159, .T. ) ;
#2080 = FACE_OUTER_BOUND ( 'NONE', #949, .T. ) ;
#2081 = DIRECTION ( 'NONE',  ( -0.000000000000000000, -0.000000000000000000, 1.000000000000000000 ) ) ;
#2082 = DIRECTION ( 'NONE',  ( -0.000000000000000000, -0.000000000000000000, -1.000000000000000000 ) ) ;
#2083 = AXIS2_PLACEMENT_3D ( 'NONE', #2371, #3832, #1226 ) ;
#2084 = VERTEX_POINT ( 'NONE', #1071 ) ;
#2085 = DIRECTION ( 'NONE',  ( -0.000000000000000000, -0.000000000000000000, -1.000000000000000000 ) ) ;
#2086 = CARTESIAN_POINT ( 'NONE',  ( -18.99999999999999645, 0.000000000000000000, -8.000000000000000000 ) ) ;
#2087 =( NAMED_UNIT ( * ) PLANE_ANGLE_UNIT ( ) SI_UNIT ( $, .RADIAN. ) );
#2088 = AXIS2_PLACEMENT_3D ( 'NONE', #1298, #991, #1031 ) ;
#2089 =( GEOMETRIC_REPRESENTATION_CONTEXT ( 3 ) GLOBAL_UNCERTAINTY_ASSIGNED_CONTEXT ( ( #3128 ) ) GLOBAL_UNIT_ASSIGNED_CONTEXT ( ( #3795, #3834, #898 ) ) REPRESENTATION_CONTEXT ( 'NONE', 'WORKASPACE' ) );
#2090 = DIRECTION ( 'NONE',  ( -1.000000000000000000, -0.000000000000000000, -0.000000000000000000 ) ) ;
#2091 = ORIENTED_EDGE ( 'NONE', *, *, #1137, .T. ) ;
#2092 = VERTEX_POINT ( 'NONE', #3122 ) ;
#2093 = CONICAL_SURFACE ( 'NONE', #2203, 1732.050807568856271, 1.047197551196592524 ) ;
#2094 = ORIENTED_EDGE ( 'NONE', *, *, #2787, .T. ) ;
#2095 = DIRECTION ( 'NONE',  ( -0.000000000000000000, -0.000000000000000000, -1.000000000000000000 ) ) ;
#2096 = ORIENTED_EDGE ( 'NONE', *, *, #1480, .T. ) ;
#2097 = CARTESIAN_POINT ( 'NONE',  ( -90.00000000000000000, 0.000000000000000000, -30.00001199999999812 ) ) ;
#2098 = ADVANCED_FACE ( 'NONE', ( #456 ), #3076, .T. ) ;
#2099 = ORIENTED_EDGE ( 'NONE', *, *, #1533, .T. ) ;
#2100 = DIRECTION ( 'NONE',  ( 0.000000000000000000, 0.000000000000000000, 1.000000000000000000 ) ) ;
#2101 = FACE_BOUND ( 'NONE', #3292, .T. ) ;
#2102 = EDGE_CURVE ( 'NONE', #2084, #916, #414, .T. ) ;
#2103 = EDGE_LOOP ( 'NONE', ( #2607, #391, #730 ) ) ;
#2104 = SURFACE_STYLE_USAGE ( .BOTH. , #3585 ) ;
#2105 = CARTESIAN_POINT ( 'NONE',  ( 1.300000000000000044, -0.7216878364870317197, -1.250000000000000000 ) ) ;
#2106 = FILL_AREA_STYLE_COLOUR ( '', #1894 ) ;
#2107 = FACE_BOUND ( 'NONE', #1253, .T. ) ;
#2108 = EDGE_LOOP ( 'NONE', ( #1482, #1942, #3607 ) ) ;
#2109 = ORIENTED_EDGE ( 'NONE', *, *, #1410, .T. ) ;
#2110 = CARTESIAN_POINT ( 'NONE',  ( 1.300000000000000044, -0.7216878364870318308, -1.250000000000000000 ) ) ;
#2112 = ORIENTED_EDGE ( 'NONE', *, *, #808, .F. ) ;
#2111 = EDGE_CURVE ( 'NONE', #1544, #1639, #1389, .T. ) ;
#2113 = DIRECTION ( 'NONE',  ( -0.000000000000000000, -0.000000000000000000, -1.000000000000000000 ) ) ;
#2114 = ORIENTED_EDGE ( 'NONE', *, *, #1698, .F. ) ;
#2115 = CARTESIAN_POINT ( 'NONE',  ( 2.021687836487040535, 2.655529440325959183E-32, -2.168404344971008868E-16 ) ) ;
#2116 = CARTESIAN_POINT ( 'NONE',  ( -3.749999999999998224, -29.76470224947664533, -30.00000000000000000 ) ) ;
#2117 = DIRECTION ( 'NONE',  ( 0.000000000000000000, 0.000000000000000000, 1.000000000000000000 ) ) ;
#2118 = CARTESIAN_POINT ( 'NONE',  ( 1.300000000000000044, 1.443375672974065216, 7.222237291452134449E-31 ) ) ;
#2119 = FACE_OUTER_BOUND ( 'NONE', #3469, .T. ) ;
#2120 = LINE ( 'NONE', #2453, #219 ) ;
#2121 = CARTESIAN_POINT ( 'NONE',  ( -21.96661513093725659, 9.224881825220236919, 2.544523588129261943E-16 ) ) ;
#2122 = ORIENTED_EDGE ( 'NONE', *, *, #719, .F. ) ;
#2123 = AXIS2_PLACEMENT_3D ( 'NONE', #3587, #1569, #2763 ) ;
#2124=STYLED_ITEM('',(#3860),#2021);
#2125 = EDGE_LOOP ( 'NONE', ( #1901, #424, #886, #3032 ) ) ;
#2126 = CARTESIAN_POINT ( 'NONE',  ( 1.649999999999999245, 2.020667218593132015E-16, -20.00000000000000000 ) ) ;
#2127 = ORIENTED_EDGE ( 'NONE', *, *, #2821, .F. ) ;
#2128 = DIRECTION ( 'NONE',  ( -0.000000000000000000, -0.000000000000000000, -1.000000000000000000 ) ) ;
#2129 = CIRCLE ( 'NONE', #443, 25.15000000000000213 ) ;
#2130 = CIRCLE ( 'NONE', #2628, 1.999999999999998224 ) ;
#2131 = CIRCLE ( 'NONE', #2010, 3.799999999999999378 ) ;
#2132 = AXIS2_PLACEMENT_3D ( 'NONE', #448, #387, #1580 ) ;
#2133 = ORIENTED_EDGE ( 'NONE', *, *, #507, .T. ) ;
#2134 = CARTESIAN_POINT ( 'NONE',  ( -23.18826319173439288, 9.737913028511604452, 0.000000000000000000 ) ) ;
#2135 = LINE ( 'NONE', #3324, #3151 ) ;
#2136 = DIRECTION ( 'NONE',  ( -0.000000000000000000, 0.000000000000000000, 1.000000000000000000 ) ) ;
#2137 = CIRCLE ( 'NONE', #3630, 2.000000000000001776 ) ;
#2138 = PLANE ( 'NONE',  #3084 ) ;
#2139 = CARTESIAN_POINT ( 'NONE',  ( 1.300000000000000044, -0.7216878364870317197, 1.250000000000000000 ) ) ;
#2140 = SURFACE_STYLE_USAGE ( .BOTH. , #3044 ) ;
#2141 = STYLED_ITEM ( 'NONE', ( #843 ), #2739 ) ;
#2142 = CIRCLE ( 'NONE', #1518, 2.700000000000000178 ) ;
#2143 = CARTESIAN_POINT ( 'NONE',  ( 10.20000000000000107, 0.000000000000000000, 0.000000000000000000 ) ) ;
#2144 = DIRECTION ( 'NONE',  ( 1.000000000000000000, 0.000000000000000000, 0.000000000000000000 ) ) ;
#2145 = COLOUR_RGB ( '',1.000000000000000000, 0.9490196078431372140, 0.9098039215686274384 ) ;
#2146 = AXIS2_PLACEMENT_3D ( 'NONE', #3805, #224, #2616 ) ;
#2147 = ORIENTED_EDGE ( 'NONE', *, *, #3609, .T. ) ;
#2148 = PLANE ( 'NONE',  #577 ) ;
#2149 = VERTEX_POINT ( 'NONE', #1937 ) ;
#2150 = AXIS2_PLACEMENT_3D ( 'NONE', #2859, #1416, #3211 ) ;
#2151 = DIRECTION ( 'NONE',  ( 0.000000000000000000, 0.000000000000000000, 1.000000000000000000 ) ) ;
#2152 = SHAPE_REPRESENTATION ( 'lid', ( #2207 ), #3459 ) ;
#2153 = EDGE_CURVE ( 'NONE', #137, #511, #1650, .T. ) ;
#2154 = CARTESIAN_POINT ( 'NONE',  ( 1.300000000000000044, 0.7216878364870328300, 1.249999999999999778 ) ) ;
#2155 = ORIENTED_EDGE ( 'NONE', *, *, #304, .T. ) ;
#2156 = DIRECTION ( 'NONE',  ( -0.000000000000000000, -0.000000000000000000, 1.000000000000000000 ) ) ;
#2157 = LINE ( 'NONE', #738, #1771 ) ;
#2158 =( NAMED_UNIT ( * ) SI_UNIT ( $, .STERADIAN. ) SOLID_ANGLE_UNIT ( ) );
#2159 = AXIS2_PLACEMENT_3D ( 'NONE', #1342, #3139, #1037 ) ;
#2160 = DIRECTION ( 'NONE',  ( 0.000000000000000000, 0.000000000000000000, 1.000000000000000000 ) ) ;
#2161 = DIRECTION ( 'NONE',  ( -0.000000000000000000, 0.000000000000000000, 1.000000000000000000 ) ) ;
#2162 =( NAMED_UNIT ( * ) PLANE_ANGLE_UNIT ( ) SI_UNIT ( $, .RADIAN. ) );
#2163 = DIRECTION ( 'NONE',  ( -0.000000000000000000, -0.000000000000000000, -1.000000000000000000 ) ) ;
#2164 = CARTESIAN_POINT ( 'NONE',  ( 0.000000000000000000, 0.000000000000000000, -20.00000000000000000 ) ) ;
#2165 = ORIENTED_EDGE ( 'NONE', *, *, #943, .F. ) ;
#2166 = ORIENTED_EDGE ( 'NONE', *, *, #866, .F. ) ;
#2167 = CYLINDRICAL_SURFACE ( 'NONE', #2822, 5.000000000000004441 ) ;
#2168 = PRODUCT ( 'o-rings series a_iso_O-ring 4x1.8-A-ISO 3601-1', 'o-rings series a_iso_O-ring 4x1.8-A-ISO 3601-1', '', ( #1449 ) ) ;
#2169 = DIRECTION ( 'NONE',  ( 0.000000000000000000, 0.000000000000000000, -1.000000000000000000 ) ) ;
#2170 = VERTEX_POINT ( 'NONE', #2502 ) ;
#2171 = CARTESIAN_POINT ( 'NONE',  ( 10.20000000000000107, 1.971681346627238735E-16, -1.610000000000000098 ) ) ;
#2172 = LINE ( 'NONE', #3360, #3575 ) ;
#2173 = CARTESIAN_POINT ( 'NONE',  ( 1.600000000000000089, 0.000000000000000000, 7.000000000000000000 ) ) ;
#2174 = CARTESIAN_POINT ( 'NONE',  ( 0.000000000000000000, 0.000000000000000000, -30.00000000000000000 ) ) ;
#2175 = EDGE_CURVE ( 'NONE', #688, #3629, #3686, .T. ) ;
#2176 = FACE_OUTER_BOUND ( 'NONE', #3034, .T. ) ;
#2177 =( NAMED_UNIT ( * ) PLANE_ANGLE_UNIT ( ) SI_UNIT ( $, .RADIAN. ) );
#2178 = EDGE_CURVE ( 'NONE', #611, #3089, #1503, .T. ) ;
#2179 = DIRECTION ( 'NONE',  ( 0.000000000000000000, 0.000000000000000000, 1.000000000000000000 ) ) ;
#2180 = CARTESIAN_POINT ( 'NONE',  ( 1.600000000000000089, 0.000000000000000000, 7.000000000000000000 ) ) ;
#2181 = ADVANCED_FACE ( 'NONE', ( #2530 ), #2839, .F. ) ;
#2182 = EDGE_CURVE ( 'NONE', #1255, #2698, #1057, .T. ) ;
#2183 = ORIENTED_EDGE ( 'NONE', *, *, #943, .T. ) ;
#2184 = ORIENTED_EDGE ( 'NONE', *, *, #2612, .F. ) ;
#2185 = LINE ( 'NONE', #987, #2266 ) ;
#2186 = AXIS2_PLACEMENT_3D ( 'NONE', #2984, #3639, #938 ) ;
#2187 = CARTESIAN_POINT ( 'NONE',  ( 3.885274725274725949, -4.336808689942017736E-16, 0.000000000000000000 ) ) ;
#2188 = ORIENTED_EDGE ( 'NONE', *, *, #1533, .F. ) ;
#2189 = DIRECTION ( 'NONE',  ( -1.000000000000000000, -0.000000000000000000, -0.000000000000000000 ) ) ;
#2190 = AXIS2_PLACEMENT_3D ( 'NONE', #3747, #792, #1977 ) ;
#2191 = DIRECTION ( 'NONE',  ( 0.000000000000000000, 0.5000000000000002220, 0.8660254037844384856 ) ) ;
#2192 = AXIS2_PLACEMENT_3D ( 'NONE', #2319, #3040, #2117 ) ;
#2193 = DIRECTION ( 'NONE',  ( -0.5890940290687334269, -0.5356142702249980792, -0.6050500627608503823 ) ) ;
#2194 = VECTOR ( 'NONE', #2908, 1000.000000000000000 ) ;
#2195 = AXIS2_PLACEMENT_3D ( 'NONE', #185, #3421, #3669 ) ;
#2196 = ORIENTED_EDGE ( 'NONE', *, *, #854, .F. ) ;
#2197 = CARTESIAN_POINT ( 'NONE',  ( 11.80999999999999872, 0.000000000000000000, 0.000000000000000000 ) ) ;
#2198 = FILL_AREA_STYLE ('',( #980 ) ) ;
#2199 = CONICAL_SURFACE ( 'NONE', #3566, 1732.050807568857181, 1.047197551196592746 ) ;
#2200 = CIRCLE ( 'NONE', #2446, 1.249999999999999778 ) ;
#2201 = LINE ( 'NONE', #1044, #2031 ) ;
#2202 = DIRECTION ( 'NONE',  ( 1.000000000000000000, 0.000000000000000000, 0.000000000000000000 ) ) ;
#2203 = AXIS2_PLACEMENT_3D ( 'NONE', #2393, #2427, #262 ) ;
#2204 = ORIENTED_EDGE ( 'NONE', *, *, #1777, .F. ) ;
#2205 = EDGE_LOOP ( 'NONE', ( #479, #579 ) ) ;
#2206 = CARTESIAN_POINT ( 'NONE',  ( -3.750000000000001776, -29.76470224947664178, 0.000000000000000000 ) ) ;
#2207 = AXIS2_PLACEMENT_3D ( 'NONE', #820, #2246, #3194 ) ;
#2208 = AXIS2_PLACEMENT_3D ( 'NONE', #697, #1591, #2762 ) ;
#2209 = PRESENTATION_LAYER_ASSIGNMENT (  '', '', ( #2338 ) ) ;
#2210 = CIRCLE ( 'NONE', #532, 1.250000000000000222 ) ;
#2211 = CARTESIAN_POINT ( 'NONE',  ( -80.00000000000000000, 0.000000000000000000, 0.000000000000000000 ) ) ;
#2212 = ORIENTED_EDGE ( 'NONE', *, *, #157, .T. ) ;
#2213 = DIRECTION ( 'NONE',  ( -1.000000000000000000, 0.000000000000000000, 0.000000000000000000 ) ) ;
#2214 = CARTESIAN_POINT ( 'NONE',  ( 8.673617379884035472E-16, 0.000000000000000000, 0.000000000000000000 ) ) ;
#2215 = CARTESIAN_POINT ( 'NONE',  ( -89.85223847358115279, -17.40498196091244409, 5.000000000000000000 ) ) ;
#2216 = EDGE_CURVE ( 'NONE', #742, #80, #2237, .T. ) ;
#2217 = VERTEX_POINT ( 'NONE', #2849 ) ;
#2218 = PRODUCT_DEFINITION_SHAPE ( 'NONE', 'NONE',  #3843 ) ;
#2219 = LINE ( 'NONE', #2819, #2894 ) ;
#2220 = ORIENTED_EDGE ( 'NONE', *, *, #2310, .T. ) ;
#2221 = FACE_OUTER_BOUND ( 'NONE', #1991, .T. ) ;
#2222 = ADVANCED_FACE ( 'NONE', ( #2467 ), #1589, .T. ) ;
#2223 =( REPRESENTATION_RELATIONSHIP ('NONE','NONE', #681, #961 ) REPRESENTATION_RELATIONSHIP_WITH_TRANSFORMATION ( #1043 )SHAPE_REPRESENTATION_RELATIONSHIP( ) );
#2224 = DIRECTION ( 'NONE',  ( 0.000000000000000000, -0.5000000000000002220, 0.8660254037844384856 ) ) ;
#2225 = CARTESIAN_POINT ( 'NONE',  ( 34.99999999999999289, 0.000000000000000000, 4.999999999999997335 ) ) ;
#2226 = VERTEX_POINT ( 'NONE', #2483 ) ;
#2227 = DIRECTION ( 'NONE',  ( 0.000000000000000000, -0.000000000000000000, -1.000000000000000000 ) ) ;
#2228 = VERTEX_POINT ( 'NONE', #1011 ) ;
#2229 = DIRECTION ( 'NONE',  ( 1.000000000000000000, 0.000000000000000000, 0.000000000000000000 ) ) ;
#2230 = ADVANCED_FACE ( 'NONE', ( #2564 ), #256, .F. ) ;
#2231 = EDGE_CURVE ( 'NONE', #261, #276, #3517, .T. ) ;
#2232 = ADVANCED_FACE ( 'NONE', ( #3491 ), #3806, .T. ) ;
#2233 = CARTESIAN_POINT ( 'NONE',  ( 8.673617379884035472E-16, 0.000000000000000000, 0.000000000000000000 ) ) ;
#2234 = ORIENTED_EDGE ( 'NONE', *, *, #1896, .T. ) ;
#2235 = DIRECTION ( 'NONE',  ( -1.000000000000000000, -0.000000000000000000, -0.000000000000000000 ) ) ;
#2236 = PLANE ( 'NONE',  #3461 ) ;
#2237 = LINE ( 'NONE', #170, #2011 ) ;
#2238 = ADVANCED_FACE ( 'NONE', ( #575, #1711 ), #3777, .F. ) ;
#2239 = EDGE_CURVE ( 'NONE', #698, #465, #3755, .T. ) ;
#2240 = LINE ( 'NONE', #2485, #1648 ) ;
#2241 = DIRECTION ( 'NONE',  ( -1.000000000000000000, 0.000000000000000000, 0.000000000000000000 ) ) ;
#2242 = DIRECTION ( 'NONE',  ( 0.000000000000000000, 0.000000000000000000, 1.000000000000000000 ) ) ;
#2243 = SURFACE_STYLE_FILL_AREA ( #1694 ) ;
#2244 = SHAPE_DEFINITION_REPRESENTATION ( #1005, #2152 ) ;
#2245 = CARTESIAN_POINT ( 'NONE',  ( 1.300000000000000044, 1.443375672974065216, 7.222237291452134449E-31 ) ) ;
#2246 = DIRECTION ( 'NONE',  ( 0.000000000000000000, 0.000000000000000000, 1.000000000000000000 ) ) ;
#2247 = VERTEX_POINT ( 'NONE', #3533 ) ;
#2248 = LINE ( 'NONE', #2596, #2627 ) ;
#2249 = EDGE_LOOP ( 'NONE', ( #503, #1048, #879 ) ) ;
#2250 = FACE_OUTER_BOUND ( 'NONE', #3080, .T. ) ;
#2251 = EDGE_CURVE ( 'NONE', #3277, #688, #1701, .T. ) ;
#2252 = CARTESIAN_POINT ( 'NONE',  ( -90.00000000000000000, -17.32050807568877815, -4.999999999999997335 ) ) ;
#2253 = VERTEX_POINT ( 'NONE', #241 ) ;
#2254 = LINE ( 'NONE', #103, #397 ) ;
#2255 = CYLINDRICAL_SURFACE ( 'NONE', #1032, 3.799999999999999378 ) ;
#2256 = DIRECTION ( 'NONE',  ( -1.000000000000000000, 0.000000000000000000, 0.000000000000000000 ) ) ;
#2257 = AXIS2_PLACEMENT_3D ( 'NONE', #1635, #2824, #1062 ) ;
#2258 = VECTOR ( 'NONE', #2782, 999.9999999999998863 ) ;
#2259 = ORIENTED_EDGE ( 'NONE', *, *, #2754, .T. ) ;
#2260 = DIRECTION ( 'NONE',  ( -1.000000000000000000, -0.000000000000000000, -0.000000000000000000 ) ) ;
#2261 = FACE_OUTER_BOUND ( 'NONE', #3247, .T. ) ;
#2262 = PRESENTATION_STYLE_ASSIGNMENT (( #725 ) ) ;
#2263 = CIRCLE ( 'NONE', #2324, 22.50000000000000355 ) ;
#2264 = AXIS2_PLACEMENT_3D ( 'NONE', #3223, #2057, #814 ) ;
#2265 = ITEM_DEFINED_TRANSFORMATION ( 'NONE', 'NONE', #2585,  #2207 ) ;
#2266 = VECTOR ( 'NONE', #2774, 999.9999999999998863 ) ;
#2267 = DIRECTION ( 'NONE',  ( 0.000000000000000000, -0.8660254037844387076, 0.5000000000000001110 ) ) ;
#2268 = SURFACE_STYLE_USAGE ( .BOTH. , #233 ) ;
#2269 = AXIS2_PLACEMENT_3D ( 'NONE', #3054, #1600, #2497 ) ;
#2270 = ORIENTED_EDGE ( 'NONE', *, *, #2521, .T. ) ;
#2271 = DIRECTION ( 'NONE',  ( 0.1250000000000000833, 0.9921567416492215186, -0.000000000000000000 ) ) ;
#2272 = ORIENTED_EDGE ( 'NONE', *, *, #1893, .T. ) ;
#2273 = DIRECTION ( 'NONE',  ( -1.000000000000000000, -0.000000000000000000, -0.000000000000000000 ) ) ;
#2274 = VECTOR ( 'NONE', #372, 999.9999999999998863 ) ;
#2275 = EDGE_CURVE ( 'NONE', #2226, #15, #2504, .T. ) ;
#2276 = UNCERTAINTY_MEASURE_WITH_UNIT (LENGTH_MEASURE( 1.000000000000000082E-05 ), #268, 'distance_accuracy_value', 'NONE');
#2277 = DIRECTION ( 'NONE',  ( 0.000000000000000000, 0.000000000000000000, 1.000000000000000000 ) ) ;
#2278 = EDGE_LOOP ( 'NONE', ( #3775, #807, #552 ) ) ;
#2279 = PLANE ( 'NONE',  #2586 ) ;
#2280 = PRESENTATION_LAYER_ASSIGNMENT (  '', '', ( #3388 ) ) ;
#2281 = AXIS2_PLACEMENT_3D ( 'NONE', #995, #661, #1847 ) ;
#2282 = CARTESIAN_POINT ( 'NONE',  ( 30.00000000000000000, 0.000000000000000000, 0.000000000000000000 ) ) ;
#2283 = EDGE_CURVE ( 'NONE', #208, #1544, #3791, .T. ) ;
#2284 = PRESENTATION_LAYER_ASSIGNMENT (  '', '', ( #1651 ) ) ;
#2285 = CIRCLE ( 'NONE', #3209, 1.250000000000000222 ) ;
#2286 = ORIENTED_EDGE ( 'NONE', *, *, #2231, .T. ) ;
#2287 = FACE_OUTER_BOUND ( 'NONE', #370, .T. ) ;
#2288 = FACE_OUTER_BOUND ( 'NONE', #1162, .T. ) ;
#2289 =( NAMED_UNIT ( * ) PLANE_ANGLE_UNIT ( ) SI_UNIT ( $, .RADIAN. ) );
#2290 = FACE_OUTER_BOUND ( 'NONE', #3628, .T. ) ;
#2291 = AXIS2_PLACEMENT_3D ( 'NONE', #3420, #2760, #2445 ) ;
#2292 = EDGE_CURVE ( 'NONE', #2698, #3067, #1757, .T. ) ;
#2293 = CARTESIAN_POINT ( 'NONE',  ( 1.649999999999998579, 2.020667218593131029E-16, -14.99999999999999645 ) ) ;
#2294 = CARTESIAN_POINT ( 'NONE',  ( -22.50000000000000355, 0.000000000000000000, 1.622657008870243228E-16 ) ) ;
#2295 = ORIENTED_EDGE ( 'NONE', *, *, #1284, .T. ) ;
#2296 = CARTESIAN_POINT ( 'NONE',  ( -80.00000000000000000, 0.000000000000000000, 0.000000000000000000 ) ) ;
#2297 = ORIENTED_EDGE ( 'NONE', *, *, #100, .F. ) ;
#2298 = DIRECTION ( 'NONE',  ( 1.000000000000000000, 0.000000000000000000, 0.000000000000000000 ) ) ;
#2299 = ORIENTED_EDGE ( 'NONE', *, *, #1638, .F. ) ;
#2300 = CARTESIAN_POINT ( 'NONE',  ( -70.00000000000000000, 0.000000000000000000, -30.00000000000000000 ) ) ;
#2301 = DIRECTION ( 'NONE',  ( -1.000000000000000000, 0.000000000000000000, 0.000000000000000000 ) ) ;
#2302 = EDGE_LOOP ( 'NONE', ( #2864, #519, #3162, #489, #82 ) ) ;
#2303 = LINE ( 'NONE', #3157, #131 ) ;
#2304 = DIRECTION ( 'NONE',  ( 0.000000000000000000, 0.000000000000000000, -1.000000000000000000 ) ) ;
#2305 = DIRECTION ( 'NONE',  ( -0.000000000000000000, 0.000000000000000000, 1.000000000000000000 ) ) ;
#2306 = CARTESIAN_POINT ( 'NONE',  ( 2.399999999999999911, 2.694222958124176020E-16, -2.199999999999999289 ) ) ;
#2307 = ORIENTED_EDGE ( 'NONE', *, *, #2423, .T. ) ;
#2308 = PLANE ( 'NONE',  #3680 ) ;
#2309 = VERTEX_POINT ( 'NONE', #1764 ) ;
#2310 = EDGE_CURVE ( 'NONE', #3181, #605, #3008, .T. ) ;
#2311 = EDGE_CURVE ( 'NONE', #3430, #964, #2602, .T. ) ;
#2312 = DIRECTION ( 'NONE',  ( 0.000000000000000000, -1.000000000000000000, 0.000000000000000000 ) ) ;
#2313 = ORIENTED_EDGE ( 'NONE', *, *, #1099, .T. ) ;
#2314 = DIRECTION ( 'NONE',  ( -1.000000000000000000, 0.000000000000000000, 0.000000000000000000 ) ) ;
#2315 = DIRECTION ( 'NONE',  ( 0.000000000000000000, 0.000000000000000000, 1.000000000000000000 ) ) ;
#2316 = ORIENTED_EDGE ( 'NONE', *, *, #2033, .F. ) ;
#2317 = DIRECTION ( 'NONE',  ( 0.000000000000000000, 0.000000000000000000, 1.000000000000000000 ) ) ;
#2318 = AXIS2_PLACEMENT_3D ( 'NONE', #1660, #3524, #2608 ) ;
#2319 = CARTESIAN_POINT ( 'NONE',  ( 2.200000000000000622, 0.000000000000000000, 0.000000000000000000 ) ) ;
#2320 = EDGE_CURVE ( 'NONE', #1107, #926, #236, .T. ) ;
#2321 = CIRCLE ( 'NONE', #3750, 0.8999999999999998002 ) ;
#2322 = EDGE_LOOP ( 'NONE', ( #1504, #3204, #113, #3726, #2540 ) ) ;
#2323 = DIRECTION ( 'NONE',  ( -0.000000000000000000, 0.4999999999999998890, -0.8660254037844387076 ) ) ;
#2324 = AXIS2_PLACEMENT_3D ( 'NONE', #731, #2227, #64 ) ;
#2325 = TOROIDAL_SURFACE ( 'NONE', #1632, 23.82500000000000284, 1.324999999999999956 ) ;
#2326 = EDGE_CURVE ( 'NONE', #1234, #1799, #379, .T. ) ;
#2327 = CIRCLE ( 'NONE', #1145, 2.700000000000000178 ) ;
#2328 = CARTESIAN_POINT ( 'NONE',  ( -4.500000000000000888, 0.000000000000000000, -24.00000000000000000 ) ) ;
#2329 = EDGE_LOOP ( 'NONE', ( #2982, #3344, #411, #1398, #3109, #3779 ) ) ;
#2330 = CIRCLE ( 'NONE', #1086, 2.199999999999999289 ) ;
#2331 = DIRECTION ( 'NONE',  ( -0.000000000000000000, 0.000000000000000000, 1.000000000000000000 ) ) ;
#2332 = ORIENTED_EDGE ( 'NONE', *, *, #162, .T. ) ;
#2333 = CARTESIAN_POINT ( 'NONE',  ( -18.99999999999999645, 0.000000000000000000, -8.000000000000000000 ) ) ;
#2334 = CARTESIAN_POINT ( 'NONE',  ( 1.600000000000000089, 3.306546357697853733E-16, -2.700000000000000178 ) ) ;
#2335 = ADVANCED_FACE ( 'NONE', ( #834 ), #3207, .T. ) ;
#2336 = ORIENTED_EDGE ( 'NONE', *, *, #3609, .F. ) ;
#2337 = CARTESIAN_POINT ( 'NONE',  ( -83.12500000000000000, -24.80391854123052653, 5.000000000000000000 ) ) ;
#2338 = STYLED_ITEM ( 'NONE', ( #2262 ), #2598 ) ;
#2339 = CIRCLE ( 'NONE', #463, 4.324969328314201000 ) ;
#2340 = ORIENTED_EDGE ( 'NONE', *, *, #804, .T. ) ;
#2341 = AXIS2_PLACEMENT_3D ( 'NONE', #3335, #705, #982 ) ;
#2342 = FACE_OUTER_BOUND ( 'NONE', #1978, .T. ) ;
#2343 = ADVANCED_FACE ( 'NONE', ( #2914 ), #2325, .T. ) ;
#2344 = DIRECTION ( 'NONE',  ( 0.000000000000000000, 0.000000000000000000, 1.000000000000000000 ) ) ;
#2345 = ORIENTED_EDGE ( 'NONE', *, *, #145, .F. ) ;
#2346 = CLOSED_SHELL ( 'NONE', ( #1846, #3208, #492, #2680, #555, #2906, #1605, #2865, #1252, #439, #2755, #608, #3146, #2514, #431, #1360, #1535, #1304, #3672, #2232, #1488, #1422, #2510, #1290, #2641, #2712, #2665 ) ) ;
#2347 = ORIENTED_EDGE ( 'NONE', *, *, #3730, .T. ) ;
#2348 = ADVANCED_FACE ( 'NONE', ( #2933 ), #205, .F. ) ;
#2349 = DIRECTION ( 'NONE',  ( 0.000000000000000000, 0.000000000000000000, 1.000000000000000000 ) ) ;
#2350 = ORIENTED_EDGE ( 'NONE', *, *, #1833, .F. ) ;
#2351 = DIRECTION ( 'NONE',  ( -1.000000000000000000, 0.000000000000000000, 0.000000000000000000 ) ) ;
#2352 = DIRECTION ( 'NONE',  ( 0.000000000000000000, 0.000000000000000000, 1.000000000000000000 ) ) ;
#2353 = EDGE_CURVE ( 'NONE', #715, #427, #2130, .T. ) ;
#2354 = APPLICATION_PROTOCOL_DEFINITION ( 'draft international standard', 'automotive_design', 1998, #3766 ) ;
#2355 = ORIENTED_EDGE ( 'NONE', *, *, #1274, .T. ) ;
#2356 = CARTESIAN_POINT ( 'NONE',  ( 2.399999999999999911, 0.000000000000000000, 0.000000000000000000 ) ) ;
#2357 = CARTESIAN_POINT ( 'NONE',  ( 2.899999999999999911, 3.551475717527323832E-16, 0.000000000000000000 ) ) ;
#2358 = EDGE_CURVE ( 'NONE', #2381, #1302, #259, .T. ) ;
#2359 = EDGE_CURVE ( 'NONE', #1737, #3824, #2441, .T. ) ;
#2360 = ORIENTED_EDGE ( 'NONE', *, *, #2521, .F. ) ;
#2361 = SURFACE_STYLE_FILL_AREA ( #2398 ) ;
#2362 = CARTESIAN_POINT ( 'NONE',  ( 10.20000000000000107, 0.000000000000000000, 0.000000000000000000 ) ) ;
#2363 = DIRECTION ( 'NONE',  ( 0.000000000000000000, 0.000000000000000000, 1.000000000000000000 ) ) ;
#2364 = ORIENTED_EDGE ( 'NONE', *, *, #1489, .F. ) ;
#2365 = VERTEX_POINT ( 'NONE', #2720 ) ;
#2366 = DIRECTION ( 'NONE',  ( -0.000000000000000000, -0.5000000000000002220, -0.8660254037844384856 ) ) ;
#2367 = ORIENTED_EDGE ( 'NONE', *, *, #1949, .F. ) ;
#2368 = CARTESIAN_POINT ( 'NONE',  ( 8.673617379884035472E-16, 1.899999999999999689, 0.000000000000000000 ) ) ;
#2369 = VERTEX_POINT ( 'NONE', #296 ) ;
#2370 = DIRECTION ( 'NONE',  ( 0.000000000000000000, 0.000000000000000000, 1.000000000000000000 ) ) ;
#2371 = CARTESIAN_POINT ( 'NONE',  ( 0.000000000000000000, 0.000000000000000000, 0.000000000000000000 ) ) ;
#2372 = FILL_AREA_STYLE_COLOUR ( '', #3681 ) ;
#2373 = VERTEX_POINT ( 'NONE', #2078 ) ;
#2374 = CARTESIAN_POINT ( 'NONE',  ( 18.99999999999999645, 2.326828918379970576E-15, -20.00000000000000000 ) ) ;
#2375 = CARTESIAN_POINT ( 'NONE',  ( -80.00000000000000000, 0.000000000000000000, -5.000000000000000000 ) ) ;
#2376 = AXIS2_PLACEMENT_3D ( 'NONE', #2006, #291, #525 ) ;
#2377 = AXIS2_PLACEMENT_3D ( 'NONE', #1560, #3650, #752 ) ;
#2378 = CONICAL_SURFACE ( 'NONE', #2435, 1732.050807568857181, 1.047197551196592746 ) ;
#2379 = EDGE_CURVE ( 'NONE', #2443, #1873, #3134, .T. ) ;
#2380 = DIRECTION ( 'NONE',  ( -0.000000000000000000, -0.000000000000000000, -1.000000000000000000 ) ) ;
#2381 = VERTEX_POINT ( 'NONE', #1524 ) ;
#2382 = CIRCLE ( 'NONE', #3070, 1.999999999999999556 ) ;
#2383 = ORIENTED_EDGE ( 'NONE', *, *, #2784, .T. ) ;
#2384 = DIRECTION ( 'NONE',  ( -1.000000000000000000, 0.000000000000000000, 0.000000000000000000 ) ) ;
#2385 = VERTEX_POINT ( 'NONE', #3296 ) ;
#2386 = AXIS2_PLACEMENT_3D ( 'NONE', #1870, #2478, #3127 ) ;
#2387 = DIRECTION ( 'NONE',  ( -0.000000000000000000, -0.4999999999999999445, -0.8660254037844387076 ) ) ;
#2388 = EDGE_CURVE ( 'NONE', #1346, #620, #1545, .T. ) ;
#2389 = PRODUCT_DEFINITION_SHAPE ( 'NONE', 'NONE',  #899 ) ;
#2390 = VECTOR ( 'NONE', #3234, 1000.000000000000000 ) ;
#2391 = ORIENTED_EDGE ( 'NONE', *, *, #2491, .F. ) ;
#2392 = CARTESIAN_POINT ( 'NONE',  ( 2.400000000000000799, 0.000000000000000000, 0.000000000000000000 ) ) ;
#2393 = CARTESIAN_POINT ( 'NONE',  ( -997.9783121635130101, 0.000000000000000000, 0.000000000000000000 ) ) ;
#2394 = LINE ( 'NONE', #1531, #1019 ) ;
#2395 = PRODUCT_DEFINITION ( 'UNKNOWN', '', #220, #477 ) ;
#2396 = AXIS2_PLACEMENT_3D ( 'NONE', #48, #1530, #3536 ) ;
#2397 = ORIENTED_EDGE ( 'NONE', *, *, #162, .F. ) ;
#2398 = FILL_AREA_STYLE ('',( #3836 ) ) ;
#2399 = CARTESIAN_POINT ( 'NONE',  ( -90.00000000000000000, 0.000000000000000000, -30.00001199999999812 ) ) ;
#2400 = SHAPE_REPRESENTATION_RELATIONSHIP ( 'NONE' , 'NONE' ,  #961, #2739 ) ;
#2401 = EDGE_CURVE ( 'NONE', #1542, #1614, #765, .T. ) ;
#2402 = AXIS2_PLACEMENT_3D ( 'NONE', #2732, #60, #2431 ) ;
#2403 = DIRECTION ( 'NONE',  ( -1.000000000000000000, -0.000000000000000000, -0.000000000000000000 ) ) ;
#2404 = ORIENTED_EDGE ( 'NONE', *, *, #1022, .F. ) ;
#2405 = VECTOR ( 'NONE', #2046, 1000.000000000000000 ) ;
#2406 = ORIENTED_EDGE ( 'NONE', *, *, #867, .F. ) ;
#2407 =( LENGTH_UNIT ( ) NAMED_UNIT ( * ) SI_UNIT ( .MILLI., .METRE. ) );
#2408 = ORIENTED_EDGE ( 'NONE', *, *, #2847, .F. ) ;
#2409 = DIRECTION ( 'NONE',  ( -0.5000000000000044409, 0.000000000000000000, 0.8660254037844360431 ) ) ;
#2410 = ORIENTED_EDGE ( 'NONE', *, *, #892, .T. ) ;
#2411 = CARTESIAN_POINT ( 'NONE',  ( 18.99999999999999645, 2.326828918379970576E-15, -8.000000000000000000 ) ) ;
#2412 = FACE_OUTER_BOUND ( 'NONE', #2958, .T. ) ;
#2413 =( NAMED_UNIT ( * ) PLANE_ANGLE_UNIT ( ) SI_UNIT ( $, .RADIAN. ) );
#2414 = CARTESIAN_POINT ( 'NONE',  ( -79.99999999999998579, -1.387778780781445676E-14, -4.999999999999990230 ) ) ;
#2415 = DIRECTION ( 'NONE',  ( -0.000000000000000000, 0.000000000000000000, 1.000000000000000000 ) ) ;
#2416 = CARTESIAN_POINT ( 'NONE',  ( 30.00000000000000711, 2.696799449851308150, 2.060606060605587597 ) ) ;
#2417 = DIRECTION ( 'NONE',  ( -1.000000000000000000, 0.000000000000000000, 0.000000000000000000 ) ) ;
#2418 = FACE_OUTER_BOUND ( 'NONE', #563, .T. ) ;
#2419 = ORIENTED_EDGE ( 'NONE', *, *, #1126, .T. ) ;
#2420 = ORIENTED_EDGE ( 'NONE', *, *, #1100, .F. ) ;
#2421 = DIRECTION ( 'NONE',  ( 0.000000000000000000, 0.000000000000000000, 1.000000000000000000 ) ) ;
#2422 = VERTEX_POINT ( 'NONE', #2699 ) ;
#2423 = EDGE_CURVE ( 'NONE', #3235, #3785, #1265, .T. ) ;
#2424 = DIRECTION ( 'NONE',  ( -0.000000000000000000, -1.000000000000000000, -0.000000000000000000 ) ) ;
#2425 = ORIENTED_EDGE ( 'NONE', *, *, #49, .T. ) ;
#2426 = PLANE ( 'NONE',  #1147 ) ;
#2427 = DIRECTION ( 'NONE',  ( -1.000000000000000000, -0.000000000000000000, -0.000000000000000000 ) ) ;
#2428 = PRODUCT_DEFINITION_SHAPE ( 'NONE', 'NONE',  #3846 ) ;
#2429 = DIRECTION ( 'NONE',  ( -0.5000000000000042188, 0.000000000000000000, 0.8660254037844361541 ) ) ;
#2430 = DIRECTION ( 'NONE',  ( 0.000000000000000000, 0.000000000000000000, 1.000000000000000000 ) ) ;
#2431 = DIRECTION ( 'NONE',  ( -0.000000000000000000, 0.000000000000000000, -1.000000000000000000 ) ) ;
#2432 = CARTESIAN_POINT ( 'NONE',  ( 1.300000000000000044, 0.7216878364870329410, 1.249999999999999778 ) ) ;
#2433 = CIRCLE ( 'NONE', #3492, 2.000000000000001776 ) ;
#2434 = EDGE_CURVE ( 'NONE', #3510, #3629, #3838, .T. ) ;
#2435 = AXIS2_PLACEMENT_3D ( 'NONE', #3697, #109, #1303 ) ;
#2436 = EDGE_LOOP ( 'NONE', ( #2406, #491, #2048, #3530, #11 ) ) ;
#2437 = SURFACE_STYLE_FILL_AREA ( #1025 ) ;
#2438 = ORIENTED_EDGE ( 'NONE', *, *, #3006, .F. ) ;
#2439 = FACE_OUTER_BOUND ( 'NONE', #475, .T. ) ;
#2440 = VECTOR ( 'NONE', #1515, 1000.000000000000000 ) ;
#2441 = CIRCLE ( 'NONE', #1441, 30.00000000000000000 ) ;
#2442 = CIRCLE ( 'NONE', #1763, 2.000000000000001776 ) ;
#2443 = VERTEX_POINT ( 'NONE', #2368 ) ;
#2444 = CARTESIAN_POINT ( 'NONE',  ( -2.000000000000000000, 0.000000000000000000, 1.102182119232618034E-16 ) ) ;
#2445 = DIRECTION ( 'NONE',  ( -1.000000000000000000, 0.000000000000000000, 0.000000000000000000 ) ) ;
#2446 = AXIS2_PLACEMENT_3D ( 'NONE', #1443, #829, #3488 ) ;
#2447 = EDGE_CURVE ( 'NONE', #3016, #3629, #967, .T. ) ;
#2448 = CARTESIAN_POINT ( 'NONE',  ( 0.000000000000000000, 0.000000000000000000, 0.000000000000000000 ) ) ;
#2449 = DIRECTION ( 'NONE',  ( 1.000000000000000000, 0.000000000000000000, -0.000000000000000000 ) ) ;
#2450 =( LENGTH_UNIT ( ) NAMED_UNIT ( * ) SI_UNIT ( .MILLI., .METRE. ) );
#2451 = AXIS2_PLACEMENT_3D ( 'NONE', #2306, #745, #2825 ) ;
#2452 = AXIS2_PLACEMENT_3D ( 'NONE', #87, #1562, #2812 ) ;
#2453 = CARTESIAN_POINT ( 'NONE',  ( 0.000000000000000000, 0.000000000000000000, 3.799999999999999378 ) ) ;
#2454 = FACE_OUTER_BOUND ( 'NONE', #1869, .T. ) ;
#2455 = CONICAL_SURFACE ( 'NONE', #3333, 1.610000000000000098, 0.7853981633974458365 ) ;
#2456 = ORIENTED_EDGE ( 'NONE', *, *, #1254, .F. ) ;
#2457 = SURFACE_SIDE_STYLE ('',( #3662 ) ) ;
#2458 = ORIENTED_EDGE ( 'NONE', *, *, #1480, .F. ) ;
#2459 = AXIS2_PLACEMENT_3D ( 'NONE', #314, #880, #2684 ) ;
#2460 = DIRECTION ( 'NONE',  ( 0.000000000000000000, 0.000000000000000000, 1.000000000000000000 ) ) ;
#2461 = ADVANCED_FACE ( 'NONE', ( #3259 ), #3013, .F. ) ;
#2462 = ADVANCED_FACE ( 'NONE', ( #2439 ), #2572, .T. ) ;
#2463 = CARTESIAN_POINT ( 'NONE',  ( -80.00000000000000000, 0.000000000000000000, 23.28427124746188781 ) ) ;
#2464 = ORIENTED_EDGE ( 'NONE', *, *, #2468, .T. ) ;
#2465 = PLANE ( 'NONE',  #2452 ) ;
#2466 = CARTESIAN_POINT ( 'NONE',  ( 1.300000000000000044, 0.000000000000000000, -1.250000000000000000 ) ) ;
#2467 = FACE_OUTER_BOUND ( 'NONE', #3546, .T. ) ;
#2468 = EDGE_CURVE ( 'NONE', #2385, #427, #32, .T. ) ;
#2469 = CARTESIAN_POINT ( 'NONE',  ( 1.999999999999998224, 2.449293598294704935E-16, -20.00000000000000355 ) ) ;
#2470 = FACE_BOUND ( 'NONE', #3831, .T. ) ;
#2471 = SURFACE_STYLE_FILL_AREA ( #1862 ) ;
#2472 = EDGE_CURVE ( 'NONE', #2909, #2646, #518, .T. ) ;
#2473 = CYLINDRICAL_SURFACE ( 'NONE', #1279, 2.000000000000001776 ) ;
#2474 = DIRECTION ( 'NONE',  ( -0.000000000000000000, 1.000000000000000000, -0.000000000000000000 ) ) ;
#2475 = ORIENTED_EDGE ( 'NONE', *, *, #612, .F. ) ;
#2476 = CARTESIAN_POINT ( 'NONE',  ( -82.50000000000000000, -19.84313483298442904, -30.00000000000000000 ) ) ;
#2477 = ORIENTED_EDGE ( 'NONE', *, *, #49, .F. ) ;
#2478 = DIRECTION ( 'NONE',  ( 0.000000000000000000, 0.000000000000000000, 1.000000000000000000 ) ) ;
#2479 = DIRECTION ( 'NONE',  ( 0.000000000000000000, 1.000000000000000000, 0.000000000000000000 ) ) ;
#2480 = ORIENTED_EDGE ( 'NONE', *, *, #2821, .T. ) ;
#2481 = PLANE ( 'NONE',  #909 ) ;
#2482 = DIRECTION ( 'NONE',  ( -1.000000000000000000, 0.000000000000000000, -0.000000000000000000 ) ) ;
#2483 = CARTESIAN_POINT ( 'NONE',  ( 1.649999999999999911, 2.020667218593133001E-16, -15.70000000000000284 ) ) ;
#2484 = VECTOR ( 'NONE', #2567, 1000.000000000000000 ) ;
#2485 = CARTESIAN_POINT ( 'NONE',  ( 1.300000000000000044, 0.7216878364870329410, 1.249999999999999778 ) ) ;
#2486 = EDGE_LOOP ( 'NONE', ( #2055, #97, #3119, #805 ) ) ;
#2487 = CARTESIAN_POINT ( 'NONE',  ( 4.499999999999993783, 5.510910596163083639E-16, -30.00000000000000000 ) ) ;
#2488 = APPLICATION_CONTEXT ( 'automotive_design' ) ;
#2489 = CYLINDRICAL_SURFACE ( 'NONE', #2871, 30.00000000000000000 ) ;
#2490 = DIRECTION ( 'NONE',  ( 1.000000000000000000, 0.000000000000000000, 0.000000000000000000 ) ) ;
#2491 = EDGE_CURVE ( 'NONE', #688, #1392, #3574, .T. ) ;
#2492 = ORIENTED_EDGE ( 'NONE', *, *, #2965, .F. ) ;
#2493 =( NAMED_UNIT ( * ) SI_UNIT ( $, .STERADIAN. ) SOLID_ANGLE_UNIT ( ) );
#2494 = ORIENTED_EDGE ( 'NONE', *, *, #3796, .T. ) ;
#2495 = CARTESIAN_POINT ( 'NONE',  ( -1.467474670309871178E-15, 0.000000000000000000, -14.00857997860452109 ) ) ;
#2496 = CIRCLE ( 'NONE', #1938, 1.250000000000000222 ) ;
#2497 = DIRECTION ( 'NONE',  ( 0.000000000000000000, 0.000000000000000000, 1.000000000000000000 ) ) ;
#2498 = ORIENTED_EDGE ( 'NONE', *, *, #2178, .F. ) ;
#2499 = EDGE_CURVE ( 'NONE', #261, #1799, #914, .T. ) ;
#2500 = AXIS2_PLACEMENT_3D ( 'NONE', #547, #2675, #1461 ) ;
#2501 = CARTESIAN_POINT ( 'NONE',  ( 2.199999999999999734, 1.999999999999999112, 0.000000000000000000 ) ) ;
#2502 = CARTESIAN_POINT ( 'NONE',  ( 1.820000000000000062, 4.653657836759941744E-16, -3.799999999999999378 ) ) ;
#2503 = VECTOR ( 'NONE', #568, 1000.000000000000227 ) ;
#2504 = CIRCLE ( 'NONE', #514, 1.649999999999999911 ) ;
#2505 = DIRECTION ( 'NONE',  ( -1.000000000000000000, -0.000000000000000000, -0.000000000000000000 ) ) ;
#2506 = CARTESIAN_POINT ( 'NONE',  ( 0.000000000000000000, 0.000000000000000000, 0.000000000000000000 ) ) ;
#2507 = DIRECTION ( 'NONE',  ( 1.000000000000000000, 0.000000000000000000, 0.000000000000000000 ) ) ;
#2508 =( NAMED_UNIT ( * ) SI_UNIT ( $, .STERADIAN. ) SOLID_ANGLE_UNIT ( ) );
#2509 = AXIS2_PLACEMENT_3D ( 'NONE', #3279, #2075, #3257 ) ;
#2510 = ADVANCED_FACE ( 'NONE', ( #614 ), #1800, .F. ) ;
#2511 = ITEM_DEFINED_TRANSFORMATION ( 'NONE', 'NONE', #2524,  #2207 ) ;
#2512 = FACE_OUTER_BOUND ( 'NONE', #3037, .T. ) ;
#2513 = CARTESIAN_POINT ( 'NONE',  ( 0.000000000000000000, 0.000000000000000000, 0.000000000000000000 ) ) ;
#2514 = ADVANCED_FACE ( 'NONE', ( #631 ), #324, .F. ) ;
#2515 = AXIS2_PLACEMENT_3D ( 'NONE', #2838, #455, #290 ) ;
#2516 = CIRCLE ( 'NONE', #332, 20.00000000000000000 ) ;
#2517 = ORIENTED_EDGE ( 'NONE', *, *, #2998, .F. ) ;
#2518 = FACE_OUTER_BOUND ( 'NONE', #135, .T. ) ;
#2519 = ORIENTED_EDGE ( 'NONE', *, *, #892, .F. ) ;
#2520 = PLANE ( 'NONE',  #3315 ) ;
#2521 = EDGE_CURVE ( 'NONE', #3156, #3065, #2808, .T. ) ;
#2522 = COLOUR_RGB ( '',1.000000000000000000, 0.9490196078431372140, 0.9098039215686274384 ) ;
#2523 = AXIS2_PLACEMENT_3D ( 'NONE', #2941, #902, #936 ) ;
#2524 = AXIS2_PLACEMENT_3D ( 'NONE', #2900, #3538, #542 ) ;
#2525 = AXIS2_PLACEMENT_3D ( 'NONE', #774, #480, #1110 ) ;
#2526 = DIRECTION ( 'NONE',  ( -1.000000000000000000, -0.000000000000000000, -0.000000000000000000 ) ) ;
#2527 = EDGE_LOOP ( 'NONE', ( #3103, #1127 ) ) ;
#2528 = CARTESIAN_POINT ( 'NONE',  ( 0.000000000000000000, 4.653657836759941744E-16, -3.799999999999999378 ) ) ;
#2529 = DIRECTION ( 'NONE',  ( -1.000000000000000000, 0.000000000000000000, -0.000000000000000000 ) ) ;
#2530 = FACE_OUTER_BOUND ( 'NONE', #1182, .T. ) ;
#2531 = PRODUCT_DEFINITION_FORMATION_WITH_SPECIFIED_SOURCE ( 'ANY', '', #1046, .NOT_KNOWN. ) ;
#2532 = DIRECTION ( 'NONE',  ( -1.000000000000000000, -0.000000000000000000, -0.000000000000000000 ) ) ;
#2533 = DIRECTION ( 'NONE',  ( -0.000000000000000000, 0.000000000000000000, 1.000000000000000000 ) ) ;
#2534 = CARTESIAN_POINT ( 'NONE',  ( 0.000000000000000000, 0.000000000000000000, -14.99999999999999645 ) ) ;
#2535 =( NAMED_UNIT ( * ) PLANE_ANGLE_UNIT ( ) SI_UNIT ( $, .RADIAN. ) );
#2536 = APPLICATION_PROTOCOL_DEFINITION ( 'draft international standard', 'automotive_design', 1998, #1619 ) ;
#2537 = CARTESIAN_POINT ( 'NONE',  ( 1.300000000000000044, -0.7216878364870317197, -1.250000000000000000 ) ) ;
#2538 = FACE_OUTER_BOUND ( 'NONE', #3569, .T. ) ;
#2539 = ADVANCED_FACE ( 'NONE', ( #3684, #425 ), #769, .T. ) ;
#2540 = ORIENTED_EDGE ( 'NONE', *, *, #2153, .F. ) ;
#2541 = DIRECTION ( 'NONE',  ( 0.000000000000000000, -0.8660254037844385966, -0.5000000000000003331 ) ) ;
#2542 = ORIENTED_EDGE ( 'NONE', *, *, #734, .F. ) ;
#2543 = CARTESIAN_POINT ( 'NONE',  ( 1.300000000000000044, -0.7216878364870319418, 1.249999999999999778 ) ) ;
#2544 = PRODUCT_DEFINITION_CONTEXT ( 'detailed design', #3766, 'design' ) ;
#2545 = DIRECTION ( 'NONE',  ( 0.000000000000000000, 0.000000000000000000, -1.000000000000000000 ) ) ;
#2546 = ORIENTED_EDGE ( 'NONE', *, *, #3332, .T. ) ;
#2547 = CARTESIAN_POINT ( 'NONE',  ( -4.374999999999999112, -34.72548595772274638, -30.00000000000000000 ) ) ;
#2548 = DIRECTION ( 'NONE',  ( -1.000000000000000000, -0.000000000000000000, -0.000000000000000000 ) ) ;
#2549 = DIRECTION ( 'NONE',  ( 0.000000000000000000, 0.000000000000000000, 1.000000000000000000 ) ) ;
#2550 = EDGE_LOOP ( 'NONE', ( #216, #1208, #3495 ) ) ;
#2551 = LINE ( 'NONE', #934, #1104 ) ;
#2552 = DIRECTION ( 'NONE',  ( -1.000000000000000000, 0.000000000000000000, 0.000000000000000000 ) ) ;
#2553 = SHAPE_DEFINITION_REPRESENTATION ( #1975, #1751 ) ;
#2554 = PLANE ( 'NONE',  #1719 ) ;
#2555 = ADVANCED_FACE ( 'NONE', ( #3053 ), #2520, .T. ) ;
#2556 = VERTEX_POINT ( 'NONE', #3648 ) ;
#2557 = DIRECTION ( 'NONE',  ( -0.9921567416492214075, 0.1250000000000000555, 0.000000000000000000 ) ) ;
#2558 = VERTEX_POINT ( 'NONE', #2495 ) ;
#2559 = FACE_OUTER_BOUND ( 'NONE', #2867, .T. ) ;
#2560 = EDGE_CURVE ( 'NONE', #973, #272, #2442, .T. ) ;
#2561 = DIRECTION ( 'NONE',  ( 0.000000000000000000, 0.000000000000000000, 1.000000000000000000 ) ) ;
#2562 = ORIENTED_EDGE ( 'NONE', *, *, #2251, .T. ) ;
#2563 = CARTESIAN_POINT ( 'NONE',  ( 0.000000000000000000, 0.000000000000000000, -24.00000000000000000 ) ) ;
#2564 = FACE_OUTER_BOUND ( 'NONE', #2566, .T. ) ;
#2565 = AXIS2_PLACEMENT_3D ( 'NONE', #2798, #3447, #3468 ) ;
#2566 = EDGE_LOOP ( 'NONE', ( #1967, #3632, #2419, #3724 ) ) ;
#2567 = DIRECTION ( 'NONE',  ( -0.8571673007021117785, 0.000000000000000000, -0.5150380749100550437 ) ) ;
#2568 = DIRECTION ( 'NONE',  ( 0.000000000000000000, -0.000000000000000000, -1.000000000000000000 ) ) ;
#2569 = AXIS2_PLACEMENT_3D ( 'NONE', #3125, #1543, #2806 ) ;
#2570 = AXIS2_PLACEMENT_3D ( 'NONE', #3155, #481, #775 ) ;
#2571 = APPLICATION_PROTOCOL_DEFINITION ( 'draft international standard', 'automotive_design', 1998, #2027 ) ;
#2572 = TOROIDAL_SURFACE ( 'NONE', #2945, 2.899999999999999911, 0.8999999999999999112 ) ;
#2573 = DIRECTION ( 'NONE',  ( -1.000000000000000000, -0.000000000000000000, -0.000000000000000000 ) ) ;
#2574 = AXIS2_PLACEMENT_3D ( 'NONE', #1067, #510, #2613 ) ;
#2575 = ORIENTED_EDGE ( 'NONE', *, *, #3359, .T. ) ;
#2576 = ORIENTED_EDGE ( 'NONE', *, *, #3273, .F. ) ;
#2577 = AXIS2_PLACEMENT_3D ( 'NONE', #816, #2002, #863 ) ;
#2578 = UNCERTAINTY_MEASURE_WITH_UNIT (LENGTH_MEASURE( 1.000000000000000082E-05 ), #2716, 'distance_accuracy_value', 'NONE');
#2579 = FACE_BOUND ( 'NONE', #1759, .T. ) ;
#2580 = ORIENTED_EDGE ( 'NONE', *, *, #3772, .T. ) ;
#2581 = DIRECTION ( 'NONE',  ( -0.000000000000000000, 0.000000000000000000, 1.000000000000000000 ) ) ;
#2582 = AXIS2_PLACEMENT_3D ( 'NONE', #2759, #3652, #1587 ) ;
#2583 = DIRECTION ( 'NONE',  ( -1.000000000000000000, -0.000000000000000000, -0.000000000000000000 ) ) ;
#2584 = ADVANCED_FACE ( 'NONE', ( #1050 ), #2167, .T. ) ;
#2585 = AXIS2_PLACEMENT_3D ( 'NONE', #582, #1805, #1508 ) ;
#2586 = AXIS2_PLACEMENT_3D ( 'NONE', #3464, #797, #3776 ) ;
#2587 = VERTEX_POINT ( 'NONE', #138 ) ;
#2588 = CARTESIAN_POINT ( 'NONE',  ( 2.000000000000001776, 2.449293598294708880E-16, -24.00000000000000000 ) ) ;
#2589 = DIRECTION ( 'NONE',  ( -1.000000000000000000, 0.000000000000000000, 0.000000000000000000 ) ) ;
#2590 = AXIS2_PLACEMENT_3D ( 'NONE', #1128, #1074, #1362 ) ;
#2591 = ADVANCED_FACE ( 'NONE', ( #3664 ), #116, .F. ) ;
#2592 = EDGE_CURVE ( 'NONE', #3645, #2149, #2185, .T. ) ;
#2593 = DIRECTION ( 'NONE',  ( -1.000000000000000000, -0.000000000000000000, -0.000000000000000000 ) ) ;
#2594 =( NAMED_UNIT ( * ) SI_UNIT ( $, .STERADIAN. ) SOLID_ANGLE_UNIT ( ) );
#2595 = VERTEX_POINT ( 'NONE', #3111 ) ;
#2596 = CARTESIAN_POINT ( 'NONE',  ( 0.000000000000000000, -1.443375672974064328, 1.278502688459867223E-18 ) ) ;
#2597 = VERTEX_POINT ( 'NONE', #3355 ) ;
#2598 = ADVANCED_BREP_SHAPE_REPRESENTATION ( '', ( #693, #2207 ), #1898 ) ;
#2599 = CARTESIAN_POINT ( 'NONE',  ( 0.000000000000000000, 0.000000000000000000, 0.000000000000000000 ) ) ;
#2600 = EDGE_LOOP ( 'NONE', ( #1767, #406, #927, #630 ) ) ;
#2601 = LINE ( 'NONE', #1688, #3027 ) ;
#2602 = LINE ( 'NONE', #1414, #1324 ) ;
#2603 = ORIENTED_EDGE ( 'NONE', *, *, #1575, .F. ) ;
#2604 = DIRECTION ( 'NONE',  ( 0.000000000000000000, -1.000000000000000000, 0.000000000000000000 ) ) ;
#2605 = CYLINDRICAL_SURFACE ( 'NONE', #2748, 2.000000000000001776 ) ;
#2606 = DIRECTION ( 'NONE',  ( 1.000000000000000000, 0.000000000000000000, 0.000000000000000000 ) ) ;
#2607 = ORIENTED_EDGE ( 'NONE', *, *, #1339, .F. ) ;
#2608 = DIRECTION ( 'NONE',  ( 1.000000000000000000, 0.000000000000000000, 0.000000000000000000 ) ) ;
#2609 = DIRECTION ( 'NONE',  ( 0.000000000000000000, 0.000000000000000000, 1.000000000000000000 ) ) ;
#2610 = DIRECTION ( 'NONE',  ( 0.000000000000000000, 0.5000000000000002220, -0.8660254037844384856 ) ) ;
#2611 = ORIENTED_EDGE ( 'NONE', *, *, #1348, .F. ) ;
#2612 = EDGE_CURVE ( 'NONE', #2422, #758, #1310, .T. ) ;
#2613 = DIRECTION ( 'NONE',  ( -1.000000000000000000, 0.000000000000000000, 0.000000000000000000 ) ) ;
#2614 = EDGE_LOOP ( 'NONE', ( #3819, #384 ) ) ;
#2615 =( REPRESENTATION_RELATIONSHIP ('NONE','NONE', #681, #2152 ) REPRESENTATION_RELATIONSHIP_WITH_TRANSFORMATION ( #2265 )SHAPE_REPRESENTATION_RELATIONSHIP( ) );
#2616 = DIRECTION ( 'NONE',  ( 0.000000000000000000, 0.000000000000000000, -1.000000000000000000 ) ) ;
#2617 = DIRECTION ( 'NONE',  ( -1.000000000000000000, -0.000000000000000000, -0.000000000000000000 ) ) ;
#2618 = EDGE_CURVE ( 'NONE', #2365, #2875, #2330, .T. ) ;
#2619 = ORIENTED_EDGE ( 'NONE', *, *, #930, .F. ) ;
#2620 = CARTESIAN_POINT ( 'NONE',  ( 1.300000000000000044, 0.7216878364870329410, -1.250000000000000000 ) ) ;
#2621 = AXIS2_PLACEMENT_3D ( 'NONE', #3424, #2568, #3720 ) ;
#2622 = DIRECTION ( 'NONE',  ( -1.000000000000000000, -1.224646799147353454E-16, 0.000000000000000000 ) ) ;
#2623 =( LENGTH_UNIT ( ) NAMED_UNIT ( * ) SI_UNIT ( .MILLI., .METRE. ) );
#2624 = PRESENTATION_LAYER_ASSIGNMENT (  '', '', ( #2124 ) ) ;
#2625 = EDGE_LOOP ( 'NONE', ( #1176, #3590 ) ) ;
#2626 = CARTESIAN_POINT ( 'NONE',  ( 1.300000000000000044, 0.7216878364870329410, -1.250000000000000000 ) ) ;
#2627 = VECTOR ( 'NONE', #234, 1000.000000000000114 ) ;
#2628 = AXIS2_PLACEMENT_3D ( 'NONE', #3549, #1181, #1239 ) ;
#2629 = EDGE_CURVE ( 'NONE', #2385, #2373, #1393, .T. ) ;
#2630 = ADVANCED_FACE ( 'NONE', ( #3727 ), #1642, .T. ) ;
#2631 = VECTOR ( 'NONE', #280, 1000.000000000000000 ) ;
#2632 = DIRECTION ( 'NONE',  ( -1.000000000000000000, 0.000000000000000000, 0.000000000000000000 ) ) ;
#2633 = VERTEX_POINT ( 'NONE', #98 ) ;
#2634 = EDGE_CURVE ( 'NONE', #691, #2633, #3375, .T. ) ;
#2635 = AXIS2_PLACEMENT_3D ( 'NONE', #3220, #795, #3168 ) ;
#2636 = ORIENTED_EDGE ( 'NONE', *, *, #1047, .T. ) ;
#2637 = EDGE_CURVE ( 'NONE', #201, #2736, #3378, .T. ) ;
#2638 = CARTESIAN_POINT ( 'NONE',  ( 12.20000000000000107, 0.000000000000000000, 0.000000000000000000 ) ) ;
#2639 = ORIENTED_EDGE ( 'NONE', *, *, #1690, .F. ) ;
#2640 = DIRECTION ( 'NONE',  ( -0.000000000000000000, 0.000000000000000000, 1.000000000000000000 ) ) ;
#2641 = ADVANCED_FACE ( 'NONE', ( #2250 ), #1294, .F. ) ;
#2642 = DIRECTION ( 'NONE',  ( 1.000000000000000000, 0.000000000000000000, -0.000000000000000000 ) ) ;
#2643 = MECHANICAL_DESIGN_GEOMETRIC_PRESENTATION_REPRESENTATION (  '', ( #3820 ), #396 ) ;
#2644 = VECTOR ( 'NONE', #674, 1000.000000000000000 ) ;
#2645 = DIRECTION ( 'NONE',  ( 0.000000000000000000, 0.000000000000000000, 1.000000000000000000 ) ) ;
#2646 = VERTEX_POINT ( 'NONE', #3458 ) ;
#2647 = DIRECTION ( 'NONE',  ( -0.000000000000000000, 0.000000000000000000, 1.000000000000000000 ) ) ;
#2648 = DIRECTION ( 'NONE',  ( -1.000000000000000000, 0.000000000000000000, 0.000000000000000000 ) ) ;
#2649 = PRESENTATION_LAYER_ASSIGNMENT (  '', '', ( #468 ) ) ;
#2650 = CIRCLE ( 'NONE', #2146, 0.2000000000000000944 ) ;
#2651 = ORIENTED_EDGE ( 'NONE', *, *, #2721, .T. ) ;
#2652 = LINE ( 'NONE', #1286, #3516 ) ;
#2653 = AXIS2_PLACEMENT_3D ( 'NONE', #1769, #2960, #285 ) ;
#2654 = DIRECTION ( 'NONE',  ( 1.000000000000000000, 0.000000000000000000, -0.000000000000000000 ) ) ;
#2655 = SURFACE_STYLE_USAGE ( .BOTH. , #1735 ) ;
#2656 = CARTESIAN_POINT ( 'NONE',  ( 0.000000000000000000, 0.000000000000000000, 0.000000000000000000 ) ) ;
#2657 = ORIENTED_EDGE ( 'NONE', *, *, #3556, .T. ) ;
#2658 = EDGE_CURVE ( 'NONE', #2217, #465, #1957, .T. ) ;
#2659 = VERTEX_POINT ( 'NONE', #1085 ) ;
#2660 = CARTESIAN_POINT ( 'NONE',  ( 1.300000000000000044, -1.443375672974063884, -3.691112476943992763E-18 ) ) ;
#2661 = ORIENTED_EDGE ( 'NONE', *, *, #3614, .F. ) ;
#2662 = DIRECTION ( 'NONE',  ( 0.000000000000000000, 0.000000000000000000, -1.000000000000000000 ) ) ;
#2663 = DIRECTION ( 'NONE',  ( -0.000000000000000000, 0.000000000000000000, 1.000000000000000000 ) ) ;
#2664 = CLOSED_SHELL ( 'NONE', ( #1859, #1866, #3029, #1419, #2939, #250, #2042, #3477, #2098, #860, #845, #3398, #1458, #1042, #3321, #3117, #2584, #3245, #1180, #3278 ) ) ;
#2665 = ADVANCED_FACE ( 'NONE', ( #2559 ), #2199, .F. ) ;
#2666 = ORIENTED_EDGE ( 'NONE', *, *, #2974, .F. ) ;
#2667 = CARTESIAN_POINT ( 'NONE',  ( -85.00000000000000000, 0.000000000000000000, 0.000000000000000000 ) ) ;
#2668 = PLANE ( 'NONE',  #93 ) ;
#2669 = CYLINDRICAL_SURFACE ( 'NONE', #20, 18.99999999999999645 ) ;
#2670 = SHAPE_REPRESENTATION_RELATIONSHIP ( 'NONE' , 'NONE' ,  #282, #1572 ) ;
#2671 = ORIENTED_EDGE ( 'NONE', *, *, #2231, .F. ) ;
#2672 = DIRECTION ( 'NONE',  ( -0.000000000000000000, -0.000000000000000000, -1.000000000000000000 ) ) ;
#2673 = CARTESIAN_POINT ( 'NONE',  ( -83.12500000000000000, -24.80391854123052653, -30.00000000000000000 ) ) ;
#2674 = ADVANCED_FACE ( 'NONE', ( #2853, #181 ), #1370, .F. ) ;
#2675 = DIRECTION ( 'NONE',  ( 1.000000000000000000, 0.000000000000000000, 0.000000000000000000 ) ) ;
#2676 = EDGE_LOOP ( 'NONE', ( #2862, #1923, #3466, #2345 ) ) ;
#2677 = ORIENTED_EDGE ( 'NONE', *, *, #26, .F. ) ;
#2678 = LINE ( 'NONE', #2718, #587 ) ;
#2679 = ORIENTED_EDGE ( 'NONE', *, *, #1205, .F. ) ;
#2680 = ADVANCED_FACE ( 'NONE', ( #2080 ), #634, .T. ) ;
#2681 = CARTESIAN_POINT ( 'NONE',  ( 1.300000000000000044, -1.443375672974063884, -3.691112476943992763E-18 ) ) ;
#2682 = ORIENTED_EDGE ( 'NONE', *, *, #1947, .F. ) ;
#2683 = DIRECTION ( 'NONE',  ( 0.000000000000000000, 0.000000000000000000, 1.000000000000000000 ) ) ;
#2684 = DIRECTION ( 'NONE',  ( 0.000000000000000000, 0.000000000000000000, 1.000000000000000000 ) ) ;
#2685 = CARTESIAN_POINT ( 'NONE',  ( 2.400000000000000799, 0.000000000000000000, 1.999999999999999112 ) ) ;
#2686 = EDGE_CURVE ( 'NONE', #1577, #2758, #1446, .T. ) ;
#2687 = ORIENTED_EDGE ( 'NONE', *, *, #3514, .F. ) ;
#2688 = PLANE ( 'NONE',  #2833 ) ;
#2689 = DIRECTION ( 'NONE',  ( -0.000000000000000000, 0.000000000000000000, 1.000000000000000000 ) ) ;
#2690 = FILL_AREA_STYLE_COLOUR ( '', #1647 ) ;
#2691 = VECTOR ( 'NONE', #819, 1000.000000000000000 ) ;
#2692 = DIRECTION ( 'NONE',  ( -0.000000000000000000, 1.000000000000000000, -0.000000000000000000 ) ) ;
#2693 = ORIENTED_EDGE ( 'NONE', *, *, #1213, .T. ) ;
#2694 = VECTOR ( 'NONE', #2786, 1000.000000000000000 ) ;
#2695 = VECTOR ( 'NONE', #2000, 1000.000000000000000 ) ;
#2696 = EDGE_LOOP ( 'NONE', ( #218, #3406, #274, #3520 ) ) ;
#2697 = LINE ( 'NONE', #2126, #29 ) ;
#2698 = VERTEX_POINT ( 'NONE', #1802 ) ;
#2699 = CARTESIAN_POINT ( 'NONE',  ( -3.749999999999998224, -29.76470224947664533, 0.000000000000000000 ) ) ;
#2700 = AXIS2_PLACEMENT_3D ( 'NONE', #85, #3096, #452 ) ;
#2701 = CONTEXT_DEPENDENT_SHAPE_REPRESENTATION ( #2765, #3031 ) ;
#2702 = ORIENTED_EDGE ( 'NONE', *, *, #3443, .F. ) ;
#2703 = DIRECTION ( 'NONE',  ( -0.000000000000000000, 0.000000000000000000, -1.000000000000000000 ) ) ;
#2704 = FACE_BOUND ( 'NONE', #1772, .T. ) ;
#2705 = PRESENTATION_STYLE_ASSIGNMENT (( #1227 ) ) ;
#2706 = DIRECTION ( 'NONE',  ( 1.000000000000000000, 5.843967824224479992E-17, 1.241531209392326468E-18 ) ) ;
#2707 = CIRCLE ( 'NONE', #1513, 22.50000000000000355 ) ;
#2708 = DIRECTION ( 'NONE',  ( 0.000000000000000000, 0.000000000000000000, 1.000000000000000000 ) ) ;
#2709 = FACE_BOUND ( 'NONE', #932, .T. ) ;
#2710 =( GEOMETRIC_REPRESENTATION_CONTEXT ( 3 ) GLOBAL_UNCERTAINTY_ASSIGNED_CONTEXT ( ( #3435 ) ) GLOBAL_UNIT_ASSIGNED_CONTEXT ( ( #3763, #3177, #2594 ) ) REPRESENTATION_CONTEXT ( 'NONE', 'WORKASPACE' ) );
#2711 = VECTOR ( 'NONE', #1935, 1000.000000000000000 ) ;
#2712 = ADVANCED_FACE ( 'NONE', ( #1505 ), #1825, .F. ) ;
#2713 =( GEOMETRIC_REPRESENTATION_CONTEXT ( 3 ) GLOBAL_UNCERTAINTY_ASSIGNED_CONTEXT ( ( #1829 ) ) GLOBAL_UNIT_ASSIGNED_CONTEXT ( ( #1383, #2535, #1364 ) ) REPRESENTATION_CONTEXT ( 'NONE', 'WORKASPACE' ) );
#2714 = CARTESIAN_POINT ( 'NONE',  ( -89.85223847358115279, -17.40498196091244409, 5.000000000000000000 ) ) ;
#2715 = ORIENTED_EDGE ( 'NONE', *, *, #667, .F. ) ;
#2716 =( LENGTH_UNIT ( ) NAMED_UNIT ( * ) SI_UNIT ( .MILLI., .METRE. ) );
#2717 = ORIENTED_EDGE ( 'NONE', *, *, #1009, .T. ) ;
#2718 = CARTESIAN_POINT ( 'NONE',  ( 1.300000000000000044, -1.443375672974064328, 1.278502688459867223E-18 ) ) ;
#2719 = ORIENTED_EDGE ( 'NONE', *, *, #2592, .T. ) ;
#2720 = CARTESIAN_POINT ( 'NONE',  ( 2.199999999999999734, 2.694222958124176020E-16, -2.199999999999999289 ) ) ;
#2721 = EDGE_CURVE ( 'NONE', #2001, #2947, #3252, .T. ) ;
#2722 = CONTEXT_DEPENDENT_SHAPE_REPRESENTATION ( #350, #3059 ) ;
#2723 = VERTEX_POINT ( 'NONE', #2134 ) ;
#2724 = DIRECTION ( 'NONE',  ( -1.000000000000000000, -0.000000000000000000, -0.000000000000000000 ) ) ;
#2725 = CARTESIAN_POINT ( 'NONE',  ( 2.899999999999999911, 3.551475717527323832E-16, 0.000000000000000000 ) ) ;
#2726 = DIRECTION ( 'NONE',  ( -0.000000000000000000, -0.5000000000000002220, -0.8660254037844384856 ) ) ;
#2727 = PRODUCT_DEFINITION_CONTEXT ( 'detailed design', #1375, 'design' ) ;
#2728 = CARTESIAN_POINT ( 'NONE',  ( 0.000000000000000000, 0.000000000000000000, -24.00000000000000000 ) ) ;
#2729 = PLANE ( 'NONE',  #1559 ) ;
#2730 =( NAMED_UNIT ( * ) PLANE_ANGLE_UNIT ( ) SI_UNIT ( $, .RADIAN. ) );
#2731 = ADVANCED_FACE ( 'NONE', ( #37 ), #2426, .T. ) ;
#2732 = CARTESIAN_POINT ( 'NONE',  ( 1.300000000000000044, -1.443375672974064328, 2.168404344971008868E-16 ) ) ;
#2733 = DIRECTION ( 'NONE',  ( -0.000000000000000000, -0.000000000000000000, -1.000000000000000000 ) ) ;
#2734 = ORIENTED_EDGE ( 'NONE', *, *, #388, .F. ) ;
#2735 = FILL_AREA_STYLE_COLOUR ( '', #3754 ) ;
#2736 = VERTEX_POINT ( 'NONE', #16 ) ;
#2737 = CARTESIAN_POINT ( 'NONE',  ( 1.300000000000000044, 0.7216878364870329410, 1.249999999999999778 ) ) ;
#2738 = EDGE_CURVE ( 'NONE', #1516, #1495, #602, .T. ) ;
#2739 = ADVANCED_BREP_SHAPE_REPRESENTATION ( '', ( #3238, #2207 ), #908 ) ;
#2740 = EDGE_LOOP ( 'NONE', ( #901, #2350 ) ) ;
#2741 = CARTESIAN_POINT ( 'NONE',  ( -4.499999999999997335, 0.000000000000000000, -30.00000000000000000 ) ) ;
#2742 = CARTESIAN_POINT ( 'NONE',  ( 1.300000000000000044, -1.443375672974064328, 1.278502688459867223E-18 ) ) ;
#2743 = DIRECTION ( 'NONE',  ( -1.000000000000000000, 0.000000000000000000, 0.000000000000000000 ) ) ;
#2744 = FACE_OUTER_BOUND ( 'NONE', #3527, .T. ) ;
#2745 = DIRECTION ( 'NONE',  ( 0.000000000000000000, 0.000000000000000000, -1.000000000000000000 ) ) ;
#2746 = AXIS2_PLACEMENT_3D ( 'NONE', #73, #3022, #2743 ) ;
#2747 = EDGE_CURVE ( 'NONE', #3559, #1302, #2994, .T. ) ;
#2748 = AXIS2_PLACEMENT_3D ( 'NONE', #838, #2061, #2648 ) ;
#2749 = ORIENTED_EDGE ( 'NONE', *, *, #727, .F. ) ;
#2750 = SURFACE_SIDE_STYLE ('',( #1556 ) ) ;
#2751 = ORIENTED_EDGE ( 'NONE', *, *, #1949, .T. ) ;
#2752 = CARTESIAN_POINT ( 'NONE',  ( 2.199999999999999734, 0.000000000000000000, 0.000000000000000000 ) ) ;
#2753 = PRESENTATION_LAYER_ASSIGNMENT (  '', '', ( #1818 ) ) ;
#2754 = EDGE_CURVE ( 'NONE', #535, #2038, #337, .T. ) ;
#2755 = ADVANCED_FACE ( 'NONE', ( #3616 ), #3038, .T. ) ;
#2756 = VECTOR ( 'NONE', #3580, 1000.000000000000000 ) ;
#2757 = CARTESIAN_POINT ( 'NONE',  ( 0.000000000000000000, 0.000000000000000000, 1.999999999999999112 ) ) ;
#2758 = VERTEX_POINT ( 'NONE', #2444 ) ;
#2759 = CARTESIAN_POINT ( 'NONE',  ( 3.885274725274726393, -8.673617379884035472E-16, 0.000000000000000000 ) ) ;
#2760 = DIRECTION ( 'NONE',  ( -0.000000000000000000, -0.000000000000000000, -1.000000000000000000 ) ) ;
#2761 = AXIS2_PLACEMENT_3D ( 'NONE', #2211, #3400, #735 ) ;
#2762 = DIRECTION ( 'NONE',  ( -1.000000000000000000, 0.000000000000000000, 0.000000000000000000 ) ) ;
#2763 = DIRECTION ( 'NONE',  ( -0.000000000000000000, 0.000000000000000000, 1.000000000000000000 ) ) ;
#2764 = AXIS2_PLACEMENT_3D ( 'NONE', #3653, #394, #3668 ) ;
#2765 =( REPRESENTATION_RELATIONSHIP ('NONE','NONE', #681, #282 ) REPRESENTATION_RELATIONSHIP_WITH_TRANSFORMATION ( #1766 )SHAPE_REPRESENTATION_RELATIONSHIP( ) );
#2766 = CIRCLE ( 'NONE', #1217, 4.499999999999993783 ) ;
#2767 = CIRCLE ( 'NONE', #1775, 2.199999999999999289 ) ;
#2768 = DIRECTION ( 'NONE',  ( 0.000000000000000000, 0.000000000000000000, 1.000000000000000000 ) ) ;
#2769 = CARTESIAN_POINT ( 'NONE',  ( -82.50000000000000000, 19.84313483298442193, 0.000000000000000000 ) ) ;
#2770 = VECTOR ( 'NONE', #962, 1000.000000000000000 ) ;
#2771 = VERTEX_POINT ( 'NONE', #2411 ) ;
#2772 = ORIENTED_EDGE ( 'NONE', *, *, #3326, .F. ) ;
#2773 = CONICAL_SURFACE ( 'NONE', #1888, 1.610000000000000098, 0.7853981633974458365 ) ;
#2774 = DIRECTION ( 'NONE',  ( -0.9921567416492215186, 0.1250000000000000833, 0.000000000000000000 ) ) ;
#2775 = DIRECTION ( 'NONE',  ( 0.000000000000000000, 0.000000000000000000, 1.000000000000000000 ) ) ;
#2776 = ORIENTED_EDGE ( 'NONE', *, *, #3332, .F. ) ;
#2777 = DIRECTION ( 'NONE',  ( 0.000000000000000000, 0.000000000000000000, 1.000000000000000000 ) ) ;
#2778 = CARTESIAN_POINT ( 'NONE',  ( -1.999999999999998224, 0.000000000000000000, -20.00000000000000355 ) ) ;
#2779 = CARTESIAN_POINT ( 'NONE',  ( 1.300000000000000044, -0.7216878364870319418, 1.249999999999999778 ) ) ;
#2780 = DIRECTION ( 'NONE',  ( -1.000000000000000000, 0.000000000000000000, 0.000000000000000000 ) ) ;
#2781 = EDGE_LOOP ( 'NONE', ( #850, #2079, #1976, #2074 ) ) ;
#2782 = DIRECTION ( 'NONE',  ( 0.9921567416492215186, 0.1250000000000001665, 0.000000000000000000 ) ) ;
#2783 = APPLICATION_PROTOCOL_DEFINITION ( 'draft international standard', 'automotive_design', 1998, #781 ) ;
#2784 = EDGE_CURVE ( 'NONE', #272, #1614, #356, .T. ) ;
#2785 = CARTESIAN_POINT ( 'NONE',  ( 0.000000000000000000, 0.000000000000000000, -20.00000000000000000 ) ) ;
#2786 = DIRECTION ( 'NONE',  ( -0.000000000000000000, -0.5000000000000001110, 0.8660254037844385966 ) ) ;
#2787 = EDGE_CURVE ( 'NONE', #2947, #2001, #1509, .T. ) ;
#2788 = VERTEX_POINT ( 'NONE', #2667 ) ;
#2789 = ORIENTED_EDGE ( 'NONE', *, *, #2787, .F. ) ;
#2790 = CARTESIAN_POINT ( 'NONE',  ( 1.300000000000000044, -0.7216878364870318308, -1.250000000000000000 ) ) ;
#2791 = LINE ( 'NONE', #2757, #386 ) ;
#2792 = EDGE_LOOP ( 'NONE', ( #3340, #2498 ) ) ;
#2793 = DIRECTION ( 'NONE',  ( 0.000000000000000000, 1.000000000000000000, 0.000000000000000000 ) ) ;
#2794 = DIRECTION ( 'NONE',  ( -1.000000000000000000, 0.000000000000000000, 0.000000000000000000 ) ) ;
#2795 = CARTESIAN_POINT ( 'NONE',  ( 30.00000000000000000, 0.000000000000000000, -30.00000000000000000 ) ) ;
#2796 = DIRECTION ( 'NONE',  ( -0.000000000000000000, -1.000000000000000000, -0.000000000000000000 ) ) ;
#2797 = ORIENTED_EDGE ( 'NONE', *, *, #3083, .F. ) ;
#2798 = CARTESIAN_POINT ( 'NONE',  ( 0.000000000000000000, 0.000000000000000000, 0.000000000000000000 ) ) ;
#2799 = EDGE_CURVE ( 'NONE', #3418, #52, #2959, .T. ) ;
#2800 = SHAPE_DEFINITION_REPRESENTATION ( #994, #282 ) ;
#2801 = CARTESIAN_POINT ( 'NONE',  ( -3.749999999999998224, 29.76470224947664533, 0.000000000000000000 ) ) ;
#2802 = DIRECTION ( 'NONE',  ( -0.9219985364506716463, 0.3871933609746164295, 0.000000000000000000 ) ) ;
#2803 = PRODUCT_DEFINITION_SHAPE ( 'NONE', 'NONE',  #1705 ) ;
#2804 = ORIENTED_EDGE ( 'NONE', *, *, #3426, .T. ) ;
#2805 = CIRCLE ( 'NONE', #3369, 5.000000000000004441 ) ;
#2806 = DIRECTION ( 'NONE',  ( 0.000000000000000000, 0.000000000000000000, -1.000000000000000000 ) ) ;
#2807 = ORIENTED_EDGE ( 'NONE', *, *, #417, .F. ) ;
#2808 = LINE ( 'NONE', #2790, #3137 ) ;
#2809 = AXIS2_PLACEMENT_3D ( 'NONE', #1185, #1986, #3497 ) ;
#2810 = DIRECTION ( 'NONE',  ( 0.000000000000000000, 1.000000000000000000, 0.000000000000000000 ) ) ;
#2811 = ORIENTED_EDGE ( 'NONE', *, *, #1536, .F. ) ;
#2812 = DIRECTION ( 'NONE',  ( 1.000000000000000000, 0.000000000000000000, 0.000000000000000000 ) ) ;
#2813 = AXIS2_PLACEMENT_3D ( 'NONE', #941, #305, #292 ) ;
#2814 = DIRECTION ( 'NONE',  ( -0.000000000000000000, -1.000000000000000000, 1.502314598737159031E-16 ) ) ;
#2815 = AXIS2_PLACEMENT_3D ( 'NONE', #2816, #147, #3716 ) ;
#2816 = CARTESIAN_POINT ( 'NONE',  ( 1.600000000000000089, 0.000000000000000000, 0.000000000000000000 ) ) ;
#2817 = CIRCLE ( 'NONE', #3314, 1.325000000000000622 ) ;
#2818 = VECTOR ( 'NONE', #1644, 1000.000000000000000 ) ;
#2819 = CARTESIAN_POINT ( 'NONE',  ( -70.00000000000000000, 0.000000000000000000, -30.00001199999999812 ) ) ;
#2820 = EDGE_LOOP ( 'NONE', ( #2188, #2355, #1934, #2364 ) ) ;
#2821 = EDGE_CURVE ( 'NONE', #3591, #2597, #1883, .T. ) ;
#2822 = AXIS2_PLACEMENT_3D ( 'NONE', #1028, #3068, #2229 ) ;
#2823 =( NAMED_UNIT ( * ) SI_UNIT ( $, .STERADIAN. ) SOLID_ANGLE_UNIT ( ) );
#2824 = DIRECTION ( 'NONE',  ( 1.000000000000000000, 0.000000000000000000, -0.000000000000000000 ) ) ;
#2825 = DIRECTION ( 'NONE',  ( 0.000000000000000000, -1.224646799147353207E-16, 1.000000000000000000 ) ) ;
#2826 = MECHANICAL_DESIGN_GEOMETRIC_PRESENTATION_REPRESENTATION (  '', ( #2141 ), #3144 ) ;
#2827 = AXIS2_PLACEMENT_3D ( 'NONE', #978, #432, #2780 ) ;
#2828 = ORIENTED_EDGE ( 'NONE', *, *, #270, .F. ) ;
#2829 = DIRECTION ( 'NONE',  ( -1.000000000000000000, 0.000000000000000000, 0.000000000000000000 ) ) ;
#2830 = ORIENTED_EDGE ( 'NONE', *, *, #26, .T. ) ;
#2831 = CARTESIAN_POINT ( 'NONE',  ( 0.000000000000000000, 0.000000000000000000, 0.000000000000000000 ) ) ;
#2832 =( GEOMETRIC_REPRESENTATION_CONTEXT ( 3 ) GLOBAL_UNCERTAINTY_ASSIGNED_CONTEXT ( ( #751 ) ) GLOBAL_UNIT_ASSIGNED_CONTEXT ( ( #1401, #3408, #817 ) ) REPRESENTATION_CONTEXT ( 'NONE', 'WORKASPACE' ) );
#2833 = AXIS2_PLACEMENT_3D ( 'NONE', #3288, #58, #641 ) ;
#2834 = VECTOR ( 'NONE', #2041, 1000.000000000000000 ) ;
#2835 = DIRECTION ( 'NONE',  ( -0.000000000000000000, -0.000000000000000000, -1.000000000000000000 ) ) ;
#2836 = ORIENTED_EDGE ( 'NONE', *, *, #382, .T. ) ;
#2837 = LINE ( 'NONE', #1282, #3145 ) ;
#2838 = CARTESIAN_POINT ( 'NONE',  ( 1.300000000000000044, 0.000000000000000000, 0.000000000000000000 ) ) ;
#2839 = CYLINDRICAL_SURFACE ( 'NONE', #2815, 2.700000000000000178 ) ;
#2840 = VERTEX_POINT ( 'NONE', #974 ) ;
#2841 = CIRCLE ( 'NONE', #664, 30.00000000000000000 ) ;
#2842 = ORIENTED_EDGE ( 'NONE', *, *, #665, .T. ) ;
#2843 = CARTESIAN_POINT ( 'NONE',  ( 0.000000000000000000, 1.443375672974065216, 7.222237291452134449E-31 ) ) ;
#2844 =( NAMED_UNIT ( * ) SI_UNIT ( $, .STERADIAN. ) SOLID_ANGLE_UNIT ( ) );
#2845 = ORIENTED_EDGE ( 'NONE', *, *, #3801, .F. ) ;
#2846 = DIRECTION ( 'NONE',  ( -1.000000000000000000, 0.000000000000000000, 0.000000000000000000 ) ) ;
#2847 = EDGE_CURVE ( 'NONE', #447, #3591, #3264, .T. ) ;
#2848 = DIRECTION ( 'NONE',  ( -0.9219985364506716463, 0.3871933609746164295, -2.048578313426146660E-17 ) ) ;
#2849 = CARTESIAN_POINT ( 'NONE',  ( 1.300000000000000044, 1.443375672974065216, 7.017607234860990640E-28 ) ) ;
#2850 = ORIENTED_EDGE ( 'NONE', *, *, #3281, .T. ) ;
#2851 = CARTESIAN_POINT ( 'NONE',  ( -3.750000000000001776, -29.76470224947664178, -30.00000000000000000 ) ) ;
#2852 = EDGE_LOOP ( 'NONE', ( #882, #3507, #2542, #571 ) ) ;
#2853 = FACE_BOUND ( 'NONE', #2625, .T. ) ;
#2854 = DIRECTION ( 'NONE',  ( 0.000000000000000000, -0.5000000000000001110, -0.8660254037844385966 ) ) ;
#2855 = ORIENTED_EDGE ( 'NONE', *, *, #855, .F. ) ;
#2856 = DIRECTION ( 'NONE',  ( -1.000000000000000000, -0.000000000000000000, -0.000000000000000000 ) ) ;
#2857 = DIRECTION ( 'NONE',  ( 0.000000000000000000, 0.000000000000000000, 1.000000000000000000 ) ) ;
#2858 = VERTEX_POINT ( 'NONE', #1768 ) ;
#2859 = CARTESIAN_POINT ( 'NONE',  ( 2.200000000000000178, 0.000000000000000000, 0.000000000000000000 ) ) ;
#2860 = DIRECTION ( 'NONE',  ( -1.000000000000000000, -0.000000000000000000, -0.000000000000000000 ) ) ;
#2861 = FACE_OUTER_BOUND ( 'NONE', #531, .T. ) ;
#2862 = ORIENTED_EDGE ( 'NONE', *, *, #1983, .F. ) ;
#2863 = DIRECTION ( 'NONE',  ( -0.000000000000000000, 0.000000000000000000, 1.000000000000000000 ) ) ;
#2864 = ORIENTED_EDGE ( 'NONE', *, *, #1348, .T. ) ;
#2865 = ADVANCED_FACE ( 'NONE', ( #3551 ), #426, .T. ) ;
#2866 = CARTESIAN_POINT ( 'NONE',  ( 0.000000000000000000, 0.000000000000000000, -8.000000000000000000 ) ) ;
#2867 = EDGE_LOOP ( 'NONE', ( #1426, #2045, #543, #1867, #3313 ) ) ;
#2868 = DIRECTION ( 'NONE',  ( -1.000000000000000000, 0.000000000000000000, 0.000000000000000000 ) ) ;
#2869 = DIRECTION ( 'NONE',  ( -1.000000000000000000, 0.000000000000000000, 0.000000000000000000 ) ) ;
#2870 = ADVANCED_BREP_SHAPE_REPRESENTATION ( '', ( #1995, #2207 ), #1040 ) ;
#2871 = AXIS2_PLACEMENT_3D ( 'NONE', #3675, #3409, #1079 ) ;
#2872 = EDGE_CURVE ( 'NONE', #2788, #757, #1311, .T. ) ;
#2873 = ADVANCED_FACE ( 'NONE', ( #1332 ), #3379, .F. ) ;
#2874 = VECTOR ( 'NONE', #2039, 1000.000000000000000 ) ;
#2875 = VERTEX_POINT ( 'NONE', #1296 ) ;
#2876 = CARTESIAN_POINT ( 'NONE',  ( -82.91666666666667140, -23.15032397181515833, 3.333333333333333037 ) ) ;
#2877 = SURFACE_STYLE_FILL_AREA ( #1400 ) ;
#2878 = SURFACE_SIDE_STYLE ('',( #2243 ) ) ;
#2879 = MECHANICAL_DESIGN_GEOMETRIC_PRESENTATION_REPRESENTATION (  '', ( #1818 ), #3376 ) ;
#2880 = AXIS2_PLACEMENT_3D ( 'NONE', #2018, #1377, #2043 ) ;
#2881 = AXIS2_PLACEMENT_3D ( 'NONE', #2187, #3712, #2810 ) ;
#2882 = CARTESIAN_POINT ( 'NONE',  ( 1.300000000000000044, 1.082531754730549300, 0.6250000000000008882 ) ) ;
#2883 =( LENGTH_UNIT ( ) NAMED_UNIT ( * ) SI_UNIT ( .MILLI., .METRE. ) );
#2884 = AXIS2_PLACEMENT_3D ( 'NONE', #2638, #1465, #1498 ) ;
#2885 = EDGE_LOOP ( 'NONE', ( #301, #307 ) ) ;
#2886 = DIRECTION ( 'NONE',  ( -0.000000000000000000, 1.000000000000000000, -0.000000000000000000 ) ) ;
#2887 = ORIENTED_EDGE ( 'NONE', *, *, #1251, .T. ) ;
#2888 = PRODUCT_RELATED_PRODUCT_CATEGORY ( 'part', '', ( #3643 ) ) ;
#2889 = VECTOR ( 'NONE', #1243, 1000.000000000000114 ) ;
#2890 = PRODUCT_DEFINITION_CONTEXT ( 'detailed design', #3415, 'design' ) ;
#2891 = CARTESIAN_POINT ( 'NONE',  ( 2.400000000000000799, 0.000000000000000000, 0.000000000000000000 ) ) ;
#2892 = ORIENTED_EDGE ( 'NONE', *, *, #727, .T. ) ;
#2893 = CARTESIAN_POINT ( 'NONE',  ( -82.50000000000000000, -19.84313483298442904, -30.00000000000000000 ) ) ;
#2894 = VECTOR ( 'NONE', #1317, 1000.000000000000000 ) ;
#2895 = CARTESIAN_POINT ( 'NONE',  ( 1.600000000000000089, 0.000000000000000000, 0.000000000000000000 ) ) ;
#2896 =( GEOMETRIC_REPRESENTATION_CONTEXT ( 3 ) GLOBAL_UNCERTAINTY_ASSIGNED_CONTEXT ( ( #660 ) ) GLOBAL_UNIT_ASSIGNED_CONTEXT ( ( #3741, #460, #2844 ) ) REPRESENTATION_CONTEXT ( 'NONE', 'WORKASPACE' ) );
#2897 = CIRCLE ( 'NONE', #3392, 30.00000000000000000 ) ;
#2898 = ORIENTED_EDGE ( 'NONE', *, *, #1245, .T. ) ;
#2899 = PLANE ( 'NONE',  #213 ) ;
#2900 = CARTESIAN_POINT ( 'NONE',  ( 0.000000000000000000, 0.000000000000000000, 0.000000000000000000 ) ) ;
#2901 = EDGE_CURVE ( 'NONE', #2253, #818, #3665, .T. ) ;
#2902 =( GEOMETRIC_REPRESENTATION_CONTEXT ( 3 ) GLOBAL_UNCERTAINTY_ASSIGNED_CONTEXT ( ( #2037 ) ) GLOBAL_UNIT_ASSIGNED_CONTEXT ( ( #3534, #174, #2823 ) ) REPRESENTATION_CONTEXT ( 'NONE', 'WORKASPACE' ) );
#2903 = ORIENTED_EDGE ( 'NONE', *, *, #566, .T. ) ;
#2904 = DIRECTION ( 'NONE',  ( 1.000000000000000000, 0.000000000000000000, 0.000000000000000000 ) ) ;
#2905 = CARTESIAN_POINT ( 'NONE',  ( 30.00000000000000000, 0.000000000000000000, -30.00000000000000000 ) ) ;
#2906 = ADVANCED_FACE ( 'NONE', ( #1006 ), #1620, .T. ) ;
#2907 = ORIENTED_EDGE ( 'NONE', *, *, #3700, .F. ) ;
#2908 = DIRECTION ( 'NONE',  ( -0.000000000000000000, -0.000000000000000000, -1.000000000000000000 ) ) ;
#2909 = VERTEX_POINT ( 'NONE', #117 ) ;
#2910 = ADVANCED_FACE ( 'NONE', ( #1355 ), #3688, .T. ) ;
#2911 = DIRECTION ( 'NONE',  ( -0.000000000000000000, -0.000000000000000000, -1.000000000000000000 ) ) ;
#2912 = VERTEX_POINT ( 'NONE', #1900 ) ;
#2913 = DIRECTION ( 'NONE',  ( 1.000000000000000000, 0.000000000000000000, 0.000000000000000000 ) ) ;
#2914 = FACE_OUTER_BOUND ( 'NONE', #1521, .T. ) ;
#2915 = ORIENTED_EDGE ( 'NONE', *, *, #2434, .T. ) ;
#2916 = CARTESIAN_POINT ( 'NONE',  ( -1.649999999999998579, 0.000000000000000000, -14.99999999999999645 ) ) ;
#2917 = DIRECTION ( 'NONE',  ( 0.000000000000000000, 0.000000000000000000, -1.000000000000000000 ) ) ;
#2918 = SURFACE_STYLE_USAGE ( .BOTH. , #2962 ) ;
#2919 = ADVANCED_FACE ( 'NONE', ( #142 ), #1872, .F. ) ;
#2920 = EDGE_CURVE ( 'NONE', #1478, #3016, #410, .T. ) ;
#2921 = EDGE_LOOP ( 'NONE', ( #2397, #3255, #3169, #3709 ) ) ;
#2922 = EDGE_CURVE ( 'NONE', #2646, #1598, #712, .T. ) ;
#2923 = DIRECTION ( 'NONE',  ( 0.000000000000000000, 0.000000000000000000, 1.000000000000000000 ) ) ;
#2924 = ADVANCED_BREP_SHAPE_REPRESENTATION ( '', ( #3290, #2207 ), #3327 ) ;
#2925 = EDGE_CURVE ( 'NONE', #1068, #143, #2137, .T. ) ;
#2926 = ADVANCED_FACE ( 'NONE', ( #672 ), #2948, .T. ) ;
#2927 = LINE ( 'NONE', #248, #323 ) ;
#2928 = ORIENTED_EDGE ( 'NONE', *, *, #2784, .F. ) ;
#2929 = ORIENTED_EDGE ( 'NONE', *, *, #719, .T. ) ;
#2930 = DIRECTION ( 'NONE',  ( -0.000000000000000000, 1.000000000000000000, 1.224646799147353207E-16 ) ) ;
#2931 = EDGE_LOOP ( 'NONE', ( #3471, #3197, #2295, #1557 ) ) ;
#2932 = CARTESIAN_POINT ( 'NONE',  ( -2.000000000000001776, 0.000000000000000000, -24.00000000000000000 ) ) ;
#2933 = FACE_OUTER_BOUND ( 'NONE', #3411, .T. ) ;
#2934 = VERTEX_POINT ( 'NONE', #166 ) ;
#2935 = DIRECTION ( 'NONE',  ( -1.000000000000000000, -0.000000000000000000, -0.000000000000000000 ) ) ;
#2936 = CARTESIAN_POINT ( 'NONE',  ( -70.00000000000000000, 0.000000000000000000, -30.00000000000000000 ) ) ;
#2937 = PRODUCT_RELATED_PRODUCT_CATEGORY ( 'part', '', ( #1046 ) ) ;
#2938 = VECTOR ( 'NONE', #19, 1000.000000000000000 ) ;
#2939 = ADVANCED_FACE ( 'NONE', ( #1856 ), #3417, .F. ) ;
#2940 = ORIENTED_EDGE ( 'NONE', *, *, #1076, .F. ) ;
#2941 = CARTESIAN_POINT ( 'NONE',  ( 0.000000000000000000, 0.000000000000000000, 0.000000000000000000 ) ) ;
#2942 = PLANE ( 'NONE',  #3124 ) ;
#2943 = VECTOR ( 'NONE', #1215, 1000.000000000000114 ) ;
#2944 = AXIS2_PLACEMENT_3D ( 'NONE', #66, #1468, #3593 ) ;
#2945 = AXIS2_PLACEMENT_3D ( 'NONE', #1196, #2113, #1855 ) ;
#2946 = CARTESIAN_POINT ( 'NONE',  ( 2.021687836487040535, 2.168404344971008868E-16, 0.000000000000000000 ) ) ;
#2947 = VERTEX_POINT ( 'NONE', #989 ) ;
#2948 = CONICAL_SURFACE ( 'NONE', #2269, 1.610000000000000098, 0.7853981633974458365 ) ;
#2949 = SHAPE_REPRESENTATION ( 'plain washer 10669 type nl_iso_ISO 10669-5.4-N', ( #2207 ), #1898 ) ;
#2950 = ORIENTED_EDGE ( 'NONE', *, *, #3613, .F. ) ;
#2951 = CARTESIAN_POINT ( 'NONE',  ( 30.00000000000000000, 0.000000000000000000, -30.00000000000000000 ) ) ;
#2952 = EDGE_LOOP ( 'NONE', ( #2299, #651, #1450, #2619 ) ) ;
#2953 = DIRECTION ( 'NONE',  ( -0.000000000000000000, -0.000000000000000000, -1.000000000000000000 ) ) ;
#2954 = DIRECTION ( 'NONE',  ( 0.000000000000000000, 0.000000000000000000, 1.000000000000000000 ) ) ;
#2955 = CIRCLE ( 'NONE', #1272, 1.899999999999999689 ) ;
#2956 = COLOUR_RGB ( '',0.8941176470588234615, 0.8941176470588234615, 0.8941176470588234615 ) ;
#2957 = CIRCLE ( 'NONE', #721, 1.999999999999999556 ) ;
#2958 = EDGE_LOOP ( 'NONE', ( #2184, #115, #186, #3573, #2575 ) ) ;
#2959 = LINE ( 'NONE', #2741, #141 ) ;
#2960 = DIRECTION ( 'NONE',  ( 0.000000000000000000, 0.000000000000000000, -1.000000000000000000 ) ) ;
#2961 = CARTESIAN_POINT ( 'NONE',  ( -87.60982564905410186, -19.87129415435180491, 5.000000000000000000 ) ) ;
#2962 = SURFACE_SIDE_STYLE ('',( #1150 ) ) ;
#2963 = STYLED_ITEM ( 'NONE', ( #287 ), #1572 ) ;
#2964 = CONICAL_SURFACE ( 'NONE', #3267, 1.649999999999998579, 1.029744258676653423 ) ;
#2965 = EDGE_CURVE ( 'NONE', #80, #2001, #2791, .T. ) ;
#2966 = EDGE_LOOP ( 'NONE', ( #3219, #1193, #483, #824, #2687 ) ) ;
#2967 = CIRCLE ( 'NONE', #2396, 1.249999999999999778 ) ;
#2968 = CARTESIAN_POINT ( 'NONE',  ( 1.300000000000000044, 0.7216878364870329410, -1.250000000000000000 ) ) ;
#2969 = EDGE_CURVE ( 'NONE', #2758, #1238, #840, .T. ) ;
#2970 = DIRECTION ( 'NONE',  ( 0.000000000000000000, 0.000000000000000000, 1.000000000000000000 ) ) ;
#2971 = EDGE_LOOP ( 'NONE', ( #3005, #108, #2828 ) ) ;
#2972 =( REPRESENTATION_RELATIONSHIP ('NONE','NONE', #681, #1751 ) REPRESENTATION_RELATIONSHIP_WITH_TRANSFORMATION ( #861 )SHAPE_REPRESENTATION_RELATIONSHIP( ) );
#2973 = EDGE_LOOP ( 'NONE', ( #2679, #3287, #1216, #171, #3011 ) ) ;
#2975 = EDGE_LOOP ( 'NONE', ( #3352, #2517, #2804, #594 ) ) ;
#2974 = EDGE_CURVE ( 'NONE', #2597, #3591, #2014, .T. ) ;
#2976 = DIRECTION ( 'NONE',  ( 1.000000000000000000, 0.000000000000000000, 0.000000000000000000 ) ) ;
#2977 = EDGE_LOOP ( 'NONE', ( #1555, #778, #711, #3550 ) ) ;
#2978 = DIRECTION ( 'NONE',  ( -0.000000000000000000, -0.000000000000000000, -1.000000000000000000 ) ) ;
#2979 = FACE_BOUND ( 'NONE', #1094, .T. ) ;
#2980 = CARTESIAN_POINT ( 'NONE',  ( 0.000000000000000000, 0.000000000000000000, -30.00000000000000000 ) ) ;
#2981 = SURFACE_STYLE_FILL_AREA ( #3228 ) ;
#2982 = ORIENTED_EDGE ( 'NONE', *, *, #164, .F. ) ;
#2983 = DIRECTION ( 'NONE',  ( -0.000000000000000000, 0.5000000000000000000, 0.8660254037844385966 ) ) ;
#2984 = CARTESIAN_POINT ( 'NONE',  ( -80.00000000000000000, 0.000000000000000000, 0.000000000000000000 ) ) ;
#2985 =( NAMED_UNIT ( * ) PLANE_ANGLE_UNIT ( ) SI_UNIT ( $, .RADIAN. ) );
#2986 = DIRECTION ( 'NONE',  ( -1.000000000000000000, 0.000000000000000000, 0.000000000000000000 ) ) ;
#2987 = ORIENTED_EDGE ( 'NONE', *, *, #1540, .F. ) ;
#2988 = EDGE_LOOP ( 'NONE', ( #1014, #2332, #3123, #1726 ) ) ;
#2989 = EDGE_CURVE ( 'NONE', #3050, #192, #3448, .T. ) ;
#2990 = FACE_OUTER_BOUND ( 'NONE', #766, .T. ) ;
#2991 = ORIENTED_EDGE ( 'NONE', *, *, #3159, .F. ) ;
#2992 = DIRECTION ( 'NONE',  ( 1.000000000000000000, 0.000000000000000000, -0.000000000000000000 ) ) ;
#2993 = VERTEX_POINT ( 'NONE', #2252 ) ;
#2994 = LINE ( 'NONE', #1843, #79 ) ;
#2995 = LINE ( 'NONE', #918, #3271 ) ;
#2996 = CYLINDRICAL_SURFACE ( 'NONE', #952, 2.000000000000001776 ) ;
#2997 = DIRECTION ( 'NONE',  ( 0.000000000000000000, 0.000000000000000000, 1.000000000000000000 ) ) ;
#2998 = EDGE_CURVE ( 'NONE', #3229, #1368, #1765, .T. ) ;
#2999 = ADVANCED_FACE ( 'NONE', ( #1708 ), #266, .F. ) ;
#3000 = DIRECTION ( 'NONE',  ( -0.000000000000000000, 1.000000000000000000, -0.000000000000000000 ) ) ;
#3001 = CYLINDRICAL_SURFACE ( 'NONE', #1496, 30.00000000000000000 ) ;
#3002 = SURFACE_STYLE_FILL_AREA ( #3588 ) ;
#3003 = TOROIDAL_SURFACE ( 'NONE', #3493, 2.899999999999999911, 0.8999999999999999112 ) ;
#3004 = CYLINDRICAL_SURFACE ( 'NONE', #3624, 30.00000000000000000 ) ;
#3005 = ORIENTED_EDGE ( 'NONE', *, *, #3564, .F. ) ;
#3006 = EDGE_CURVE ( 'NONE', #2858, #535, #2200, .T. ) ;
#3007 = AXIS2_PLACEMENT_3D ( 'NONE', #1754, #2380, #1886 ) ;
#3008 = CIRCLE ( 'NONE', #204, 2.199999999999999289 ) ;
#3009 = EDGE_LOOP ( 'NONE', ( #1787, #1424, #3478, #2147, #3748 ) ) ;
#3010 = CARTESIAN_POINT ( 'NONE',  ( 22.50000000000000355, 2.755455298081545172E-15, 0.000000000000000000 ) ) ;
#3011 = ORIENTED_EDGE ( 'NONE', *, *, #486, .F. ) ;
#3012 = AXIS2_PLACEMENT_3D ( 'NONE', #1242, #2978, #2 ) ;
#3013 = CYLINDRICAL_SURFACE ( 'NONE', #770, 1.999999999999999112 ) ;
#3014 = AXIS2_PLACEMENT_3D ( 'NONE', #2891, #253, #2561 ) ;
#3015 = PRODUCT_RELATED_PRODUCT_CATEGORY ( 'part', '', ( #3567 ) ) ;
#3016 = VERTEX_POINT ( 'NONE', #3152 ) ;
#3017 = DIRECTION ( 'NONE',  ( -1.000000000000000000, 0.000000000000000000, 0.000000000000000000 ) ) ;
#3018 = CARTESIAN_POINT ( 'NONE',  ( -80.00000000000000000, 0.000000000000000000, 0.000000000000000000 ) ) ;
#3019 = AXIS2_PLACEMENT_3D ( 'NONE', #22, #2415, #3304 ) ;
#3020 = AXIS2_PLACEMENT_3D ( 'NONE', #1851, #3660, #363 ) ;
#3021 = CARTESIAN_POINT ( 'NONE',  ( 12.20000000000000107, 0.000000000000000000, 0.000000000000000000 ) ) ;
#3022 = DIRECTION ( 'NONE',  ( -0.000000000000000000, -0.000000000000000000, -1.000000000000000000 ) ) ;
#3023 =( NAMED_UNIT ( * ) SI_UNIT ( $, .STERADIAN. ) SOLID_ANGLE_UNIT ( ) );
#3024 = APPLICATION_CONTEXT ( 'automotive_design' ) ;
#3025 = AXIS2_PLACEMENT_3D ( 'NONE', #1204, #920, #522 ) ;
#3026=STYLED_ITEM('',(#3881),#693);
#3027 = VECTOR ( 'NONE', #2868, 1000.000000000000000 ) ;
#3028 = PLANE ( 'NONE',  #2402 ) ;
#3029 = ADVANCED_FACE ( 'NONE', ( #222 ), #238, .T. ) ;
#3030 = LINE ( 'NONE', #1613, #2022 ) ;
#3031 = PRODUCT_DEFINITION_SHAPE ( 'NONE', 'NONE',  #3845 ) ;
#3032 = ORIENTED_EDGE ( 'NONE', *, *, #589, .F. ) ;
#3033 = FACE_OUTER_BOUND ( 'NONE', #2977, .T. ) ;
#3034 = EDGE_LOOP ( 'NONE', ( #1723, #2259, #13, #1683, #2360 ) ) ;
#3035 = DIRECTION ( 'NONE',  ( 0.000000000000000000, 0.000000000000000000, 1.000000000000000000 ) ) ;
#3036 = ADVANCED_FACE ( 'NONE', ( #478 ), #211, .T. ) ;
#3037 = EDGE_LOOP ( 'NONE', ( #226, #2112, #2715 ) ) ;
#3038 = CYLINDRICAL_SURFACE ( 'NONE', #1570, 1.999999999999999112 ) ;
#3039 = CARTESIAN_POINT ( 'NONE',  ( 0.000000000000000000, 0.000000000000000000, -20.00000000000000355 ) ) ;
#3040 = DIRECTION ( 'NONE',  ( -1.000000000000000000, -0.000000000000000000, -0.000000000000000000 ) ) ;
#3041 = DIRECTION ( 'NONE',  ( -0.000000000000000000, 0.000000000000000000, 1.000000000000000000 ) ) ;
#3042 = ADVANCED_FACE ( 'NONE', ( #1122 ), #3731, .T. ) ;
#3043 = CARTESIAN_POINT ( 'NONE',  ( -3.749999999999998224, -29.76470224947664533, -30.00000000000000000 ) ) ;
#3044 = SURFACE_SIDE_STYLE ('',( #3105 ) ) ;
#3045 = EDGE_CURVE ( 'NONE', #3181, #2947, #197, .T. ) ;
#3046 = CARTESIAN_POINT ( 'NONE',  ( 0.000000000000000000, 2.449293598294705428E-16, -1.999999999999999112 ) ) ;
#3047 = CARTESIAN_POINT ( 'NONE',  ( -3.749999999999998224, 29.76470224947664533, -30.00000000000000000 ) ) ;
#3048 = ADVANCED_FACE ( 'NONE', ( #551 ), #3694, .F. ) ;
#3049 = EDGE_CURVE ( 'NONE', #1107, #910, #1511, .T. ) ;
#3050 = VERTEX_POINT ( 'NONE', #1979 ) ;
#3051 = FILL_AREA_STYLE_COLOUR ( '', #3439 ) ;
#3052 = VERTEX_POINT ( 'NONE', #1373 ) ;
#3053 = FACE_OUTER_BOUND ( 'NONE', #2103, .T. ) ;
#3054 = CARTESIAN_POINT ( 'NONE',  ( 10.20000000000000107, 0.000000000000000000, 0.000000000000000000 ) ) ;
#3055 = ORIENTED_EDGE ( 'NONE', *, *, #3120, .T. ) ;
#3056 = CARTESIAN_POINT ( 'NONE',  ( 1.649999999999998579, 2.020667218593131029E-16, -14.99999999999999645 ) ) ;
#3057 = DIRECTION ( 'NONE',  ( -0.5000000000000044409, 1.060575238724903587E-16, -0.8660254037844360431 ) ) ;
#3058 = SURFACE_STYLE_FILL_AREA ( #676 ) ;
#3059 = PRODUCT_DEFINITION_SHAPE ( 'NONE', 'NONE',  #3844 ) ;
#3060 = DIRECTION ( 'NONE',  ( -0.000000000000000000, -1.000000000000000000, 1.502314598737159031E-16 ) ) ;
#3061 = CARTESIAN_POINT ( 'NONE',  ( -82.00000000000000000, 0.000000000000000000, -5.000000000000000000 ) ) ;
#3062 = DIRECTION ( 'NONE',  ( -1.000000000000000000, -0.000000000000000000, -0.000000000000000000 ) ) ;
#3063 = CYLINDRICAL_SURFACE ( 'NONE', #3020, 5.000000000000004441 ) ;
#3064 = AXIS2_PLACEMENT_3D ( 'NONE', #762, #440, #3723 ) ;
#3065 = VERTEX_POINT ( 'NONE', #3788 ) ;
#3066 = SURFACE_STYLE_USAGE ( .BOTH. , #3090 ) ;
#3067 = VERTEX_POINT ( 'NONE', #1739 ) ;
#3068 = DIRECTION ( 'NONE',  ( -0.000000000000000000, -0.000000000000000000, 1.000000000000000000 ) ) ;
#3069 = PRESENTATION_LAYER_ASSIGNMENT (  '', '', ( #1878 ) ) ;
#3070 = AXIS2_PLACEMENT_3D ( 'NONE', #1359, #3383, #1877 ) ;
#3071 = VECTOR ( 'NONE', #1529, 1000.000000000000000 ) ;
#3072 = DIRECTION ( 'NONE',  ( -0.000000000000000000, -0.000000000000000000, -1.000000000000000000 ) ) ;
#3073 = EDGE_LOOP ( 'NONE', ( #3814, #3544, #524, #366, #67 ) ) ;
#3074 = DIRECTION ( 'NONE',  ( -1.000000000000000000, -0.000000000000000000, -0.000000000000000000 ) ) ;
#3075 = CARTESIAN_POINT ( 'NONE',  ( 0.000000000000000000, -0.7216878364870318308, 1.249999999999999778 ) ) ;
#3076 = PLANE ( 'NONE',  #704 ) ;
#3077 = EDGE_CURVE ( 'NONE', #605, #2001, #3570, .T. ) ;
#3078 = AXIS2_PLACEMENT_3D ( 'NONE', #1053, #714, #1917 ) ;
#3079 = DIRECTION ( 'NONE',  ( -0.000000000000000000, -0.5000000000000001110, 0.8660254037844385966 ) ) ;
#3080 = EDGE_LOOP ( 'NONE', ( #2336, #1474, #2316 ) ) ;
#3081 = DIRECTION ( 'NONE',  ( -0.000000000000000000, 0.5000000000000000000, 0.8660254037844385966 ) ) ;
#3082 = AXIS2_PLACEMENT_3D ( 'NONE', #3039, #992, #2794 ) ;
#3083 = EDGE_CURVE ( 'NONE', #102, #742, #3760, .T. ) ;
#3084 = AXIS2_PLACEMENT_3D ( 'NONE', #621, #3330, #1748 ) ;
#3085 = DIRECTION ( 'NONE',  ( -1.000000000000000000, -0.000000000000000000, -0.000000000000000000 ) ) ;
#3086 = LINE ( 'NONE', #1574, #832 ) ;
#3087 = PRODUCT_RELATED_PRODUCT_CATEGORY ( 'part', '', ( #1795 ) ) ;
#3088 = VECTOR ( 'NONE', #646, 1000.000000000000000 ) ;
#3089 = VERTEX_POINT ( 'NONE', #3473 ) ;
#3090 = SURFACE_SIDE_STYLE ('',( #2437 ) ) ;
#3091 = VERTEX_POINT ( 'NONE', #1686 ) ;
#3092 = CIRCLE ( 'NONE', #3260, 0.8999999999999998002 ) ;
#3093 = CARTESIAN_POINT ( 'NONE',  ( 1.300000000000000044, -1.443375672974064328, 2.168404344971008868E-16 ) ) ;
#3094 = PRODUCT_DEFINITION_SHAPE ( 'NONE', 'NONE',  #3840 ) ;
#3095 = EDGE_CURVE ( 'NONE', #1105, #2771, #1387, .T. ) ;
#3096 = DIRECTION ( 'NONE',  ( -0.000000000000000000, -0.000000000000000000, -1.000000000000000000 ) ) ;
#3097 = EDGE_LOOP ( 'NONE', ( #3187, #1499, #3485, #1123 ) ) ;
#3098 = FACE_OUTER_BOUND ( 'NONE', #2302, .T. ) ;
#3099 = DIRECTION ( 'NONE',  ( -0.9921567416492215186, 0.1250000000000000833, 0.000000000000000000 ) ) ;
#3100 = LINE ( 'NONE', #3692, #3377 ) ;
#3101 = APPLICATION_CONTEXT ( 'automotive_design' ) ;
#3102 = CARTESIAN_POINT ( 'NONE',  ( 3.885274725274725949, -4.336808689942017736E-16, 0.000000000000000000 ) ) ;
#3103 = ORIENTED_EDGE ( 'NONE', *, *, #1893, .F. ) ;
#3104 = CARTESIAN_POINT ( 'NONE',  ( -25.15000000000000213, 0.000000000000000000, 0.000000000000000000 ) ) ;
#3105 = SURFACE_STYLE_FILL_AREA ( #2198 ) ;
#3106 = APPLICATION_PROTOCOL_DEFINITION ( 'draft international standard', 'automotive_design', 1998, #1566 ) ;
#3107 = FACE_OUTER_BOUND ( 'NONE', #3380, .T. ) ;
#3108 = DIRECTION ( 'NONE',  ( 0.000000000000000000, 0.000000000000000000, 1.000000000000000000 ) ) ;
#3109 = ORIENTED_EDGE ( 'NONE', *, *, #1213, .F. ) ;
#3110 = ORIENTED_EDGE ( 'NONE', *, *, #3658, .T. ) ;
#3111 = CARTESIAN_POINT ( 'NONE',  ( -75.00000000000000000, 6.123233995736772199E-16, -4.999999999999997335 ) ) ;
#3112 = ORIENTED_EDGE ( 'NONE', *, *, #2468, .F. ) ;
#3113 = LINE ( 'NONE', #1008, #971 ) ;
#3114 = LINE ( 'NONE', #1860, #1285 ) ;
#3115 = DIRECTION ( 'NONE',  ( -1.000000000000000000, -0.000000000000000000, -0.000000000000000000 ) ) ;
#3116 = ADVANCED_BREP_SHAPE_REPRESENTATION ( '', ( #2021, #2207 ), #3459 ) ;
#3117 = ADVANCED_FACE ( 'NONE', ( #2579, #1141 ), #3774, .F. ) ;
#3118 = DIRECTION ( 'NONE',  ( 1.000000000000000000, 0.000000000000000000, 0.000000000000000000 ) ) ;
#3119 = ORIENTED_EDGE ( 'NONE', *, *, #1489, .T. ) ;
#3120 = EDGE_CURVE ( 'NONE', #1281, #1639, #3511, .T. ) ;
#3121 = LINE ( 'NONE', #1679, #659 ) ;
#3122 = CARTESIAN_POINT ( 'NONE',  ( 1.820000000000000062, -3.799999999999999378, -4.653657836759940757E-16 ) ) ;
#3123 = ORIENTED_EDGE ( 'NONE', *, *, #3765, .T. ) ;
#3124 = AXIS2_PLACEMENT_3D ( 'NONE', #3272, #2654, #1171 ) ;
#3125 = CARTESIAN_POINT ( 'NONE',  ( 1.600000000000000089, 0.000000000000000000, 0.000000000000000000 ) ) ;
#3126 = EDGE_LOOP ( 'NONE', ( #2347, #1914, #2109, #1064, #1616 ) ) ;
#3127 = DIRECTION ( 'NONE',  ( 1.000000000000000000, 0.000000000000000000, -0.000000000000000000 ) ) ;
#3128 = UNCERTAINTY_MEASURE_WITH_UNIT (LENGTH_MEASURE( 1.000000000000000082E-05 ), #3795, 'distance_accuracy_value', 'NONE');
#3129 = DIRECTION ( 'NONE',  ( 0.000000000000000000, -1.000000000000000000, 0.000000000000000000 ) ) ;
#3130 = ORIENTED_EDGE ( 'NONE', *, *, #3729, .F. ) ;
#3131 = DIRECTION ( 'NONE',  ( 1.000000000000000000, 0.000000000000000000, 0.000000000000000000 ) ) ;
#3132 = VECTOR ( 'NONE', #1736, 1000.000000000000000 ) ;
#3133 = DIRECTION ( 'NONE',  ( 0.000000000000000000, 0.000000000000000000, 1.000000000000000000 ) ) ;
#3134 = CIRCLE ( 'NONE', #3625, 1.899999999999999689 ) ;
#3135 = CARTESIAN_POINT ( 'NONE',  ( 20.00000000000000000, 0.000000000000000000, -20.00000000000000000 ) ) ;
#3136 = EDGE_CURVE ( 'NONE', #1729, #1187, #2678, .T. ) ;
#3137 = VECTOR ( 'NONE', #3434, 1000.000000000000000 ) ;
#3138 = ORIENTED_EDGE ( 'NONE', *, *, #78, .F. ) ;
#3139 = DIRECTION ( 'NONE',  ( 0.000000000000000000, 0.000000000000000000, 1.000000000000000000 ) ) ;
#3140 = CARTESIAN_POINT ( 'NONE',  ( 1.820000000000000062, 4.653657836759941744E-16, -3.799999999999999378 ) ) ;
#3141 = AXIS2_PLACEMENT_3D ( 'NONE', #1933, #3129, #2169 ) ;
#3142 = PLANE ( 'NONE',  #2318 ) ;
#3143 =( NAMED_UNIT ( * ) PLANE_ANGLE_UNIT ( ) SI_UNIT ( $, .RADIAN. ) );
#3144 =( GEOMETRIC_REPRESENTATION_CONTEXT ( 3 ) GLOBAL_UNCERTAINTY_ASSIGNED_CONTEXT ( ( #2276 ) ) GLOBAL_UNIT_ASSIGNED_CONTEXT ( ( #268, #2087, #3525 ) ) REPRESENTATION_CONTEXT ( 'NONE', 'WORKASPACE' ) );
#3145 = VECTOR ( 'NONE', #3381, 1000.000000000000000 ) ;
#3146 = ADVANCED_FACE ( 'NONE', ( #2990 ), #308, .F. ) ;
#3147 = VERTEX_POINT ( 'NONE', #889 ) ;
#3148 = ORIENTED_EDGE ( 'NONE', *, *, #1327, .F. ) ;
#3149 = CARTESIAN_POINT ( 'NONE',  ( -997.9783121635130101, 0.000000000000000000, 0.000000000000000000 ) ) ;
#3150 = CIRCLE ( 'NONE', #2525, 1.324999999999999956 ) ;
#3151 = VECTOR ( 'NONE', #1167, 1000.000000000000000 ) ;
#3152 = CARTESIAN_POINT ( 'NONE',  ( 1.300000000000000044, 0.7216878364870328300, 1.249999999999999778 ) ) ;
#3153 = ORIENTED_EDGE ( 'NONE', *, *, #802, .T. ) ;
#3154 = DIRECTION ( 'NONE',  ( 1.000000000000000000, 0.000000000000000000, 0.000000000000000000 ) ) ;
#3155 = CARTESIAN_POINT ( 'NONE',  ( 0.000000000000000000, 0.000000000000000000, -20.00000000000000000 ) ) ;
#3156 = VERTEX_POINT ( 'NONE', #2110 ) ;
#3157 = CARTESIAN_POINT ( 'NONE',  ( -75.00000000000000000, 0.000000000000000000, -5.000000000000000000 ) ) ;
#3158 = CARTESIAN_POINT ( 'NONE',  ( -70.00000000000000000, -21.41798680385620202, -4.999999999999997335 ) ) ;
#3159 = EDGE_CURVE ( 'NONE', #3824, #2309, #945, .T. ) ;
#3160 = CARTESIAN_POINT ( 'NONE',  ( 1.300000000000000044, 0.000000000000000000, 0.000000000000000000 ) ) ;
#3161 = CYLINDRICAL_SURFACE ( 'NONE', #720, 30.00000000000000000 ) ;
#3162 = ORIENTED_EDGE ( 'NONE', *, *, #1205, .T. ) ;
#3163 = DIRECTION ( 'NONE',  ( -0.000000000000000000, -0.000000000000000000, -1.000000000000000000 ) ) ;
#3164 = ORIENTED_EDGE ( 'NONE', *, *, #3006, .T. ) ;
#3165 = EDGE_CURVE ( 'NONE', #1368, #2226, #2697, .T. ) ;
#3166 = EDGE_CURVE ( 'NONE', #1346, #929, #12, .T. ) ;
#3167 = UNCERTAINTY_MEASURE_WITH_UNIT (LENGTH_MEASURE( 1.000000000000000082E-05 ), #1308, 'distance_accuracy_value', 'NONE');
#3168 = DIRECTION ( 'NONE',  ( 0.000000000000000000, 0.000000000000000000, 1.000000000000000000 ) ) ;
#3169 = ORIENTED_EDGE ( 'NONE', *, *, #2799, .T. ) ;
#3170 = APPLICATION_CONTEXT ( 'automotive_design' ) ;
#3171 = LINE ( 'NONE', #536, #1221 ) ;
#3172 = CARTESIAN_POINT ( 'NONE',  ( 34.99999999999999289, 0.000000000000000000, 4.999999999999997335 ) ) ;
#3173 = ORIENTED_EDGE ( 'NONE', *, *, #2747, .F. ) ;
#3174 = DIRECTION ( 'NONE',  ( -0.000000000000000000, 0.000000000000000000, 1.000000000000000000 ) ) ;
#3175 = DIRECTION ( 'NONE',  ( 0.000000000000000000, 0.000000000000000000, 1.000000000000000000 ) ) ;
#3176 = CARTESIAN_POINT ( 'NONE',  ( 1.300000000000000044, 0.000000000000000000, 0.000000000000000000 ) ) ;
#3177 =( NAMED_UNIT ( * ) PLANE_ANGLE_UNIT ( ) SI_UNIT ( $, .RADIAN. ) );
#3178 = ORIENTED_EDGE ( 'NONE', *, *, #549, .F. ) ;
#3179 = CARTESIAN_POINT ( 'NONE',  ( -70.00000000000000000, 0.000000000000000000, -30.00001199999999812 ) ) ;
#3180 = ORIENTED_EDGE ( 'NONE', *, *, #3649, .F. ) ;
#3181 = VERTEX_POINT ( 'NONE', #1177 ) ;
#3182 = CARTESIAN_POINT ( 'NONE',  ( 1.300000000000000044, 0.000000000000000000, 0.000000000000000000 ) ) ;
#3183 = DIRECTION ( 'NONE',  ( -1.000000000000000000, -0.000000000000000000, -0.000000000000000000 ) ) ;
#3184 = AXIS2_PLACEMENT_3D ( 'NONE', #3506, #2541, #2610 ) ;
#3185 = AXIS2_PLACEMENT_3D ( 'NONE', #801, #3537, #1472 ) ;
#3186 = EDGE_CURVE ( 'NONE', #1392, #818, #3317, .T. ) ;
#3187 = ORIENTED_EDGE ( 'NONE', *, *, #1371, .F. ) ;
#3188 = CARTESIAN_POINT ( 'NONE',  ( -4.499999999999993783, 0.000000000000000000, -30.00000000000000000 ) ) ;
#3189 = FACE_OUTER_BOUND ( 'NONE', #986, .T. ) ;
#3190 = CIRCLE ( 'NONE', #643, 1.610000000000000098 ) ;
#3191 = AXIS2_PLACEMENT_3D ( 'NONE', #3442, #1624, #2857 ) ;
#3192 = ORIENTED_EDGE ( 'NONE', *, *, #855, .T. ) ;
#3193 = CARTESIAN_POINT ( 'NONE',  ( 0.000000000000000000, 0.000000000000000000, -30.00000000000000000 ) ) ;
#3194 = DIRECTION ( 'NONE',  ( 1.000000000000000000, 0.000000000000000000, 0.000000000000000000 ) ) ;
#3195 = ADVANCED_FACE ( 'NONE', ( #51 ), #1237, .T. ) ;
#3196 = AXIS2_PLACEMENT_3D ( 'NONE', #390, #2277, #493 ) ;
#3197 = ORIENTED_EDGE ( 'NONE', *, *, #2499, .F. ) ;
#3198 = PLANE ( 'NONE',  #3184 ) ;
#3199 = EDGE_LOOP ( 'NONE', ( #709, #2212, #3413 ) ) ;
#3200 = AXIS2_PLACEMENT_3D ( 'NONE', #169, #1936, #3133 ) ;
#3201 = UNCERTAINTY_MEASURE_WITH_UNIT (LENGTH_MEASURE( 1.000000000000000082E-05 ), #2883, 'distance_accuracy_value', 'NONE');
#3202 = EDGE_CURVE ( 'NONE', #1238, #2758, #1087, .T. ) ;
#3203 = DIRECTION ( 'NONE',  ( -1.000000000000000000, 0.000000000000000000, 0.000000000000000000 ) ) ;
#3204 = ORIENTED_EDGE ( 'NONE', *, *, #667, .T. ) ;
#3205 = CARTESIAN_POINT ( 'NONE',  ( -82.50000000000000000, 19.84313483298442193, -30.00000000000000000 ) ) ;
#3206 = VECTOR ( 'NONE', #2160, 1000.000000000000000 ) ;
#3207 = CYLINDRICAL_SURFACE ( 'NONE', #640, 7.000000000000000000 ) ;
#3208 = ADVANCED_FACE ( 'NONE', ( #3033 ), #1707, .F. ) ;
#3209 = AXIS2_PLACEMENT_3D ( 'NONE', #3182, #2856, #1961 ) ;
#3210 = VERTEX_POINT ( 'NONE', #1481 ) ;
#3211 = DIRECTION ( 'NONE',  ( 0.000000000000000000, 0.000000000000000000, 1.000000000000000000 ) ) ;
#3212 = EDGE_CURVE ( 'NONE', #3089, #611, #1448, .T. ) ;
#3213 = MANIFOLD_SOLID_BREP ( 'Sweep1', #615 ) ;
#3214 = EDGE_LOOP ( 'NONE', ( #3732, #281, #1479 ) ) ;
#3215 = FACE_OUTER_BOUND ( 'NONE', #3474, .T. ) ;
#3216 =( REPRESENTATION_RELATIONSHIP ('NONE','NONE', #681, #2949 ) REPRESENTATION_RELATIONSHIP_WITH_TRANSFORMATION ( #311 )SHAPE_REPRESENTATION_RELATIONSHIP( ) );
#3217 = CARTESIAN_POINT ( 'NONE',  ( -2.000000000000001776, 0.000000000000000000, -30.00000000000000000 ) ) ;
#3218 = ORIENTED_EDGE ( 'NONE', *, *, #2618, .T. ) ;
#3219 = ORIENTED_EDGE ( 'NONE', *, *, #2447, .T. ) ;
#3220 = CARTESIAN_POINT ( 'NONE',  ( 10.20000000000000107, 0.000000000000000000, 0.000000000000000000 ) ) ;
#3221 = ORIENTED_EDGE ( 'NONE', *, *, #382, .F. ) ;
#3222 = CARTESIAN_POINT ( 'NONE',  ( -80.00000000000000000, 0.000000000000000000, 0.000000000000000000 ) ) ;
#3223 = CARTESIAN_POINT ( 'NONE',  ( 2.399999999999999911, 0.000000000000000000, 0.000000000000000000 ) ) ;
#3224 = EDGE_CURVE ( 'NONE', #2993, #573, #826, .T. ) ;
#3225 = EDGE_LOOP ( 'NONE', ( #1469, #2196, #3745, #3647 ) ) ;
#3226 = CARTESIAN_POINT ( 'NONE',  ( 1.600000000000000089, 3.306546357697853733E-16, -2.700000000000000178 ) ) ;
#3227 = DIRECTION ( 'NONE',  ( 0.000000000000000000, 0.000000000000000000, 1.000000000000000000 ) ) ;
#3228 = FILL_AREA_STYLE ('',( #1677 ) ) ;
#3229 = VERTEX_POINT ( 'NONE', #928 ) ;
#3230 = CARTESIAN_POINT ( 'NONE',  ( 2.000000000000000000, 2.449293598294706414E-16, 0.000000000000000000 ) ) ;
#3231 = CARTESIAN_POINT ( 'NONE',  ( 1.300000000000000044, 1.443375672974065216, 7.222237291452134449E-31 ) ) ;
#3232 = ORIENTED_EDGE ( 'NONE', *, *, #604, .F. ) ;
#3233 = ORIENTED_EDGE ( 'NONE', *, *, #1251, .F. ) ;
#3234 = DIRECTION ( 'NONE',  ( -0.000000000000000000, -1.000000000000000000, 1.502314598737159031E-16 ) ) ;
#3235 = VERTEX_POINT ( 'NONE', #3010 ) ;
#3236 = LINE ( 'NONE', #1762, #3583 ) ;
#3237 = DIRECTION ( 'NONE',  ( -0.000000000000000000, -0.000000000000000000, 1.000000000000000000 ) ) ;
#3238 = MANIFOLD_SOLID_BREP ( 'M4 Tapped Hole1', #1229 ) ;
#3239 = ITEM_DEFINED_TRANSFORMATION ( 'NONE', 'NONE', #1223,  #2207 ) ;
#3240 = ORIENTED_EDGE ( 'NONE', *, *, #3276, .T. ) ;
#3241 = CARTESIAN_POINT ( 'NONE',  ( -20.74496707014011676, 8.711850621928869387, 0.000000000000000000 ) ) ;
#3242 = CIRCLE ( 'NONE', #1384, 34.99999999999999289 ) ;
#3243 = CARTESIAN_POINT ( 'NONE',  ( 2.400000000000000799, 0.000000000000000000, 0.000000000000000000 ) ) ;
#3244 = DIRECTION ( 'NONE',  ( 0.000000000000000000, 0.000000000000000000, 1.000000000000000000 ) ) ;
#3245 = ADVANCED_FACE ( 'NONE', ( #965, #407 ), #329, .T. ) ;
#3246 = CIRCLE ( 'NONE', #2809, 5.000000000000004441 ) ;
#3247 = EDGE_LOOP ( 'NONE', ( #2016, #2987, #628 ) ) ;
#3248 = CARTESIAN_POINT ( 'NONE',  ( 2.021687836487040535, 0.000000000000000000, 2.168404344971008868E-16 ) ) ;
#3249 = LINE ( 'NONE', #1189, #18 ) ;
#3250 = CIRCLE ( 'NONE', #894, 20.00000000000000355 ) ;
#3251 = AXIS2_PLACEMENT_3D ( 'NONE', #1034, #3404, #1921 ) ;
#3252 = CIRCLE ( 'NONE', #584, 1.999999999999999112 ) ;
#3253 = MANIFOLD_SOLID_BREP ( 'Hex', #1541 ) ;
#3254 = DIRECTION ( 'NONE',  ( 1.000000000000000000, 0.000000000000000000, 0.000000000000000000 ) ) ;
#3255 = ORIENTED_EDGE ( 'NONE', *, *, #977, .F. ) ;
#3256 = ORIENTED_EDGE ( 'NONE', *, *, #2592, .F. ) ;
#3257 = DIRECTION ( 'NONE',  ( 0.000000000000000000, 0.000000000000000000, -1.000000000000000000 ) ) ;
#3258 = EDGE_LOOP ( 'NONE', ( #585, #2410, #2749, #1224 ) ) ;
#3259 = FACE_OUTER_BOUND ( 'NONE', #1089, .T. ) ;
#3260 = AXIS2_PLACEMENT_3D ( 'NONE', #2725, #618, #17 ) ;
#3261 = AXIS2_PLACEMENT_3D ( 'NONE', #488, #3482, #526 ) ;
#3262 = CIRCLE ( 'NONE', #2281, 1.249999999999999778 ) ;
#3263 = ORIENTED_EDGE ( 'NONE', *, *, #134, .F. ) ;
#3264 = LINE ( 'NONE', #3345, #3687 ) ;
#3265 = CARTESIAN_POINT ( 'NONE',  ( 0.000000000000000000, 0.000000000000000000, 0.000000000000000000 ) ) ;
#3266 =( LENGTH_UNIT ( ) NAMED_UNIT ( * ) SI_UNIT ( .MILLI., .METRE. ) );
#3267 = AXIS2_PLACEMENT_3D ( 'NONE', #574, #348, #682 ) ;
#3268 = ORIENTED_EDGE ( 'NONE', *, *, #2969, .F. ) ;
#3269 = LINE ( 'NONE', #2118, #1717 ) ;
#3270 = PRODUCT_DEFINITION_FORMATION_WITH_SPECIFIED_SOURCE ( 'ANY', '', #3612, .NOT_KNOWN. ) ;
#3271 = VECTOR ( 'NONE', #2081, 1000.000000000000000 ) ;
#3272 = CARTESIAN_POINT ( 'NONE',  ( 1.300000000000000044, -1.443375672974064328, 2.168404344971008868E-16 ) ) ;
#3273 = EDGE_CURVE ( 'NONE', #671, #385, #2263, .T. ) ;
#3274 = CARTESIAN_POINT ( 'NONE',  ( -4.374999999999999112, -34.72548595772274638, 4.999999999999997335 ) ) ;
#3275 = ORIENTED_EDGE ( 'NONE', *, *, #1052, .F. ) ;
#3276 = EDGE_CURVE ( 'NONE', #1281, #208, #1440, .T. ) ;
#3277 = VERTEX_POINT ( 'NONE', #136 ) ;
#3278 = ADVANCED_FACE ( 'NONE', ( #2518 ), #2148, .F. ) ;
#3279 = CARTESIAN_POINT ( 'NONE',  ( -2.899999999999999911, 0.000000000000000000, 0.000000000000000000 ) ) ;
#3280 = ORIENTED_EDGE ( 'NONE', *, *, #2434, .F. ) ;
#3281 = EDGE_CURVE ( 'NONE', #2012, #821, #3353, .T. ) ;
#3282 = DIRECTION ( 'NONE',  ( 0.000000000000000000, 0.000000000000000000, 1.000000000000000000 ) ) ;
#3283 = ORIENTED_EDGE ( 'NONE', *, *, #3606, .F. ) ;
#3284 = DIRECTION ( 'NONE',  ( 1.000000000000000000, 0.000000000000000000, 0.000000000000000000 ) ) ;
#3285 = DIRECTION ( 'NONE',  ( 1.000000000000000000, 0.000000000000000000, 0.000000000000000000 ) ) ;
#3286 = DIRECTION ( 'NONE',  ( -1.241531209392323001E-18, -5.843967824224479992E-17, 1.000000000000000000 ) ) ;
#3287 = ORIENTED_EDGE ( 'NONE', *, *, #2358, .T. ) ;
#3288 = CARTESIAN_POINT ( 'NONE',  ( -3.750000000000001776, -29.76470224947664178, -30.00000000000000000 ) ) ;
#3289 = FACE_OUTER_BOUND ( 'NONE', #242, .T. ) ;
#3290 = MANIFOLD_SOLID_BREP ( 'Sweep1', #358 ) ;
#3291 = PLANE ( 'NONE',  #2500 ) ;
#3292 = EDGE_LOOP ( 'NONE', ( #1462, #1160 ) ) ;
#3293 = ORIENTED_EDGE ( 'NONE', *, *, #977, .T. ) ;
#3294 = DIRECTION ( 'NONE',  ( -1.000000000000000000, 0.000000000000000000, 0.000000000000000000 ) ) ;
#3295 = ORIENTED_EDGE ( 'NONE', *, *, #1626, .T. ) ;
#3296 = CARTESIAN_POINT ( 'NONE',  ( -2.000000000000000000, 0.000000000000000000, -15.70000000000000284 ) ) ;
#3297 = PRODUCT_DEFINITION_SHAPE ( 'NONE', 'NONE',  #3842 ) ;
#3298 = ORIENTED_EDGE ( 'NONE', *, *, #3186, .F. ) ;
#3299 = DIRECTION ( 'NONE',  ( 0.000000000000000000, 0.000000000000000000, 1.000000000000000000 ) ) ;
#3300 = CARTESIAN_POINT ( 'NONE',  ( 2.200000000000000622, 1.999999999999999112, 0.000000000000000000 ) ) ;
#3301 =( LENGTH_UNIT ( ) NAMED_UNIT ( * ) SI_UNIT ( .MILLI., .METRE. ) );
#3302 = EDGE_CURVE ( 'NONE', #2633, #1495, #1853, .T. ) ;
#3303 = VECTOR ( 'NONE', #434, 1000.000000000000000 ) ;
#3304 = DIRECTION ( 'NONE',  ( 1.000000000000000000, 0.000000000000000000, 0.000000000000000000 ) ) ;
#3305 = DIRECTION ( 'NONE',  ( -1.000000000000000000, 0.000000000000000000, -0.000000000000000000 ) ) ;
#3306 =( NAMED_UNIT ( * ) SI_UNIT ( $, .STERADIAN. ) SOLID_ANGLE_UNIT ( ) );
#3307 = AXIS2_PLACEMENT_3D ( 'NONE', #743, #1924, #1343 ) ;
#3308 = ADVANCED_FACE ( 'NONE', ( #2035 ), #849, .F. ) ;
#3309 = CIRCLE ( 'NONE', #1631, 3.799999999999999378 ) ;
#3310 = AXIS2_PLACEMENT_3D ( 'NONE', #2779, #105, #1300 ) ;
#3311 = LINE ( 'NONE', #3046, #3088 ) ;
#3312 = CARTESIAN_POINT ( 'NONE',  ( -75.00000000000000000, 6.123233995736772199E-16, 0.001000000000000132727 ) ) ;
#3313 = ORIENTED_EDGE ( 'NONE', *, *, #1327, .T. ) ;
#3314 = AXIS2_PLACEMENT_3D ( 'NONE', #2121, #1021, #2802 ) ;
#3315 = AXIS2_PLACEMENT_3D ( 'NONE', #2543, #1915, #2460 ) ;
#3316 = ORIENTED_EDGE ( 'NONE', *, *, #157, .F. ) ;
#3317 = LINE ( 'NONE', #2660, #1210 ) ;
#3318 = EDGE_LOOP ( 'NONE', ( #1743, #1621, #2657, #180 ) ) ;
#3319 = PRESENTATION_LAYER_ASSIGNMENT (  '', '', ( #960 ) ) ;
#3320 = DIRECTION ( 'NONE',  ( -0.000000000000000000, -0.000000000000000000, -1.000000000000000000 ) ) ;
#3321 = ADVANCED_FACE ( 'NONE', ( #194 ), #3769, .T. ) ;
#3322 = ORIENTED_EDGE ( 'NONE', *, *, #422, .T. ) ;
#3323 = CARTESIAN_POINT ( 'NONE',  ( 1.300000000000000044, -0.7216878364870319418, 1.249999999999999778 ) ) ;
#3324 = CARTESIAN_POINT ( 'NONE',  ( -78.00000000000000000, 2.449293598294708880E-16, -5.000000000000000000 ) ) ;
#3325 = CYLINDRICAL_SURFACE ( 'NONE', #3623, 1.649999999999999245 ) ;
#3326 = EDGE_CURVE ( 'NONE', #2993, #276, #1352, .T. ) ;
#3327 =( GEOMETRIC_REPRESENTATION_CONTEXT ( 3 ) GLOBAL_UNCERTAINTY_ASSIGNED_CONTEXT ( ( #2578 ) ) GLOBAL_UNIT_ASSIGNED_CONTEXT ( ( #2716, #2985, #1810 ) ) REPRESENTATION_CONTEXT ( 'NONE', 'WORKASPACE' ) );
#3328 = PRESENTATION_LAYER_ASSIGNMENT (  '', '', ( #3026 ) ) ;
#3329 = ADVANCED_FACE ( 'NONE', ( #446 ), #1682, .T. ) ;
#3330 = DIRECTION ( 'NONE',  ( 0.000000000000000000, 0.8660254037844387076, 0.4999999999999998890 ) ) ;
#3331 = DIRECTION ( 'NONE',  ( -0.000000000000000000, 0.000000000000000000, 1.000000000000000000 ) ) ;
#3332 = EDGE_CURVE ( 'NONE', #2556, #3430, #2248, .T. ) ;
#3333 = AXIS2_PLACEMENT_3D ( 'NONE', #2143, #3062, #2179 ) ;
#3334 = PRODUCT_DEFINITION_FORMATION_WITH_SPECIFIED_SOURCE ( 'ANY', '', #343, .NOT_KNOWN. ) ;
#3335 = CARTESIAN_POINT ( 'NONE',  ( 3.885274725274726393, -8.673617379884035472E-16, 0.000000000000000000 ) ) ;
#3336 = DIRECTION ( 'NONE',  ( -0.000000000000000000, -0.000000000000000000, 1.000000000000000000 ) ) ;
#3337 = PRODUCT_DEFINITION_SHAPE ( 'NONE', 'NONE',  #1232 ) ;
#3338 = ORIENTED_EDGE ( 'NONE', *, *, #196, .F. ) ;
#3339 = DIRECTION ( 'NONE',  ( 0.000000000000000000, 0.000000000000000000, 1.000000000000000000 ) ) ;
#3340 = ORIENTED_EDGE ( 'NONE', *, *, #3212, .F. ) ;
#3341 = CLOSED_SHELL ( 'NONE', ( #2919, #1988, #3308, #2230, #1406, #1746, #1663, #678, #361, #1436, #2591, #3542, #1929, #2539, #3717, #937, #389, #3329, #1667, #2873, #3722, #1887, #2238, #1140 ) ) ;
#3342 = CARTESIAN_POINT ( 'NONE',  ( 0.000000000000000000, 0.000000000000000000, -20.00000000000000000 ) ) ;
#3343 = CARTESIAN_POINT ( 'NONE',  ( 0.000000000000000000, 0.000000000000000000, -24.00000000000000000 ) ) ;
#3344 = ORIENTED_EDGE ( 'NONE', *, *, #517, .F. ) ;
#3345 = CARTESIAN_POINT ( 'NONE',  ( -85.00000000000000000, 6.123233995736771213E-16, -5.000000000000000000 ) ) ;
#3346 = LINE ( 'NONE', #1603, #88 ) ;
#3347 = CARTESIAN_POINT ( 'NONE',  ( 12.20000000000000107, 1.971681346627238735E-16, -1.610000000000000098 ) ) ;
#3348 = CARTESIAN_POINT ( 'NONE',  ( -83.12500000000000000, -24.80391854123052653, -30.00000000000000000 ) ) ;
#3349 = CARTESIAN_POINT ( 'NONE',  ( 1.300000000000000044, -0.7216878364870317197, 1.250000000000000000 ) ) ;
#3350 = LINE ( 'NONE', #1850, #2770 ) ;
#3351 = DIRECTION ( 'NONE',  ( 0.000000000000000000, 0.000000000000000000, -1.000000000000000000 ) ) ;
#3352 = ORIENTED_EDGE ( 'NONE', *, *, #3165, .F. ) ;
#3353 = LINE ( 'NONE', #2476, #1567 ) ;
#3354 = ORIENTED_EDGE ( 'NONE', *, *, #1657, .F. ) ;
#3355 = CARTESIAN_POINT ( 'NONE',  ( -75.00000000000000000, 0.000000000000000000, 0.000000000000000000 ) ) ;
#3356 = DIRECTION ( 'NONE',  ( -0.000000000000000000, -0.4999999999999999445, -0.8660254037844387076 ) ) ;
#3357 = ORIENTED_EDGE ( 'NONE', *, *, #1284, .F. ) ;
#3358 = FACE_OUTER_BOUND ( 'NONE', #2971, .T. ) ;
#3359 = EDGE_CURVE ( 'NONE', #3615, #758, #3250, .T. ) ;
#3360 = CARTESIAN_POINT ( 'NONE',  ( 0.000000000000000000, 4.653657836759941744E-16, -3.799999999999999378 ) ) ;
#3361 = DIRECTION ( 'NONE',  ( -0.7071067811865492381, 0.000000000000000000, 0.7071067811865457964 ) ) ;
#3362 =( REPRESENTATION_RELATIONSHIP ('NONE','NONE', #681, #159 ) REPRESENTATION_RELATIONSHIP_WITH_TRANSFORMATION ( #2511 )SHAPE_REPRESENTATION_RELATIONSHIP( ) );
#3363 = DIRECTION ( 'NONE',  ( 0.000000000000000000, 0.000000000000000000, 1.000000000000000000 ) ) ;
#3364 = DIRECTION ( 'NONE',  ( -1.000000000000000000, 0.000000000000000000, 0.000000000000000000 ) ) ;
#3365 =( NAMED_UNIT ( * ) PLANE_ANGLE_UNIT ( ) SI_UNIT ( $, .RADIAN. ) );
#3366 = PRODUCT_DEFINITION ( 'UNKNOWN', '', #2034, #1685 ) ;
#3367 = DIRECTION ( 'NONE',  ( 0.000000000000000000, 0.000000000000000000, -1.000000000000000000 ) ) ;
#3368 = CARTESIAN_POINT ( 'NONE',  ( 1.300000000000000044, 0.000000000000000000, 1.249999999999999778 ) ) ;
#3369 = AXIS2_PLACEMENT_3D ( 'NONE', #2375, #3837, #3783 ) ;
#3370 = ADVANCED_FACE ( 'NONE', ( #1391 ), #3198, .T. ) ;
#3371 = AXIS2_PLACEMENT_3D ( 'NONE', #629, #345, #875 ) ;
#3372 = CIRCLE ( 'NONE', #442, 3.799999999999999378 ) ;
#3373 = ORIENTED_EDGE ( 'NONE', *, *, #3359, .F. ) ;
#3374 = ORIENTED_EDGE ( 'NONE', *, *, #1092, .T. ) ;
#3375 = LINE ( 'NONE', #3414, #25 ) ;
#3376 =( GEOMETRIC_REPRESENTATION_CONTEXT ( 3 ) GLOBAL_UNCERTAINTY_ASSIGNED_CONTEXT ( ( #3711 ) ) GLOBAL_UNIT_ASSIGNED_CONTEXT ( ( #823, #1703, #1367 ) ) REPRESENTATION_CONTEXT ( 'NONE', 'WORKASPACE' ) );
#3377 = VECTOR ( 'NONE', #3735, 1000.000000000000000 ) ;
#3378 = CIRCLE ( 'NONE', #3444, 7.000000000000000000 ) ;
#3379 = CYLINDRICAL_SURFACE ( 'NONE', #207, 9.999999999999994671 ) ;
#3380 = EDGE_LOOP ( 'NONE', ( #2772, #1490, #2693, #3373, #36, #1747 ) ) ;
#3381 = DIRECTION ( 'NONE',  ( 0.000000000000000000, 0.000000000000000000, 1.000000000000000000 ) ) ;
#3382 = FACE_BOUND ( 'NONE', #246, .T. ) ;
#3383 = DIRECTION ( 'NONE',  ( -1.000000000000000000, -0.000000000000000000, -0.000000000000000000 ) ) ;
#3384 = AXIS2_PLACEMENT_3D ( 'NONE', #3547, #2384, #650 ) ;
#3385 = CARTESIAN_POINT ( 'NONE',  ( 10.20000000000000107, 0.000000000000000000, 1.610000000000000098 ) ) ;
#3386 = ORIENTED_EDGE ( 'NONE', *, *, #2102, .T. ) ;
#3387 = DIRECTION ( 'NONE',  ( -0.000000000000000000, 0.000000000000000000, 1.000000000000000000 ) ) ;
#3388 = STYLED_ITEM ( 'NONE', ( #1974 ), #791 ) ;
#3389 = AXIS2_PLACEMENT_3D ( 'NONE', #6, #2085, #1230 ) ;
#3390 = DIRECTION ( 'NONE',  ( -1.000000000000000000, -0.000000000000000000, -0.000000000000000000 ) ) ;
#3391 = LINE ( 'NONE', #3312, #1336 ) ;
#3392 = AXIS2_PLACEMENT_3D ( 'NONE', #1102, #190, #803 ) ;
#3393 = EDGE_LOOP ( 'NONE', ( #888, #1191, #1601, #3338, #944 ) ) ;
#3394 = EDGE_LOOP ( 'NONE', ( #2458, #773, #2480, #2297 ) ) ;
#3395 = AXIS2_PLACEMENT_3D ( 'NONE', #870, #1493, #8 ) ;
#3396 = CARTESIAN_POINT ( 'NONE',  ( 0.000000000000000000, 0.000000000000000000, 0.000000000000000000 ) ) ;
#3397 = PRODUCT ( 'socket button head screw_iso_ISO 7380 - M4 x 8 - 8N', 'socket button head screw_iso_ISO 7380 - M4 x 8 - 8N', '', ( #1061 ) ) ;
#3398 = ADVANCED_FACE ( 'NONE', ( #1106 ), #2308, .F. ) ;
#3399 = CIRCLE ( 'NONE', #2159, 2.000000000000001776 ) ;
#3400 = DIRECTION ( 'NONE',  ( 0.000000000000000000, -0.000000000000000000, -1.000000000000000000 ) ) ;
#3401 = ORIENTED_EDGE ( 'NONE', *, *, #1066, .T. ) ;
#3402 = FACE_BOUND ( 'NONE', #2527, .T. ) ;
#3403 = FACE_OUTER_BOUND ( 'NONE', #2076, .T. ) ;
#3404 = DIRECTION ( 'NONE',  ( -1.000000000000000000, -0.000000000000000000, -0.000000000000000000 ) ) ;
#3405 = DIRECTION ( 'NONE',  ( -1.000000000000000000, 0.000000000000000000, 0.000000000000000000 ) ) ;
#3406 = ORIENTED_EDGE ( 'NONE', *, *, #275, .F. ) ;
#3407 = CYLINDRICAL_SURFACE ( 'NONE', #3307, 2.000000000000001776 ) ;
#3408 =( NAMED_UNIT ( * ) PLANE_ANGLE_UNIT ( ) SI_UNIT ( $, .RADIAN. ) );
#3409 = DIRECTION ( 'NONE',  ( -0.000000000000000000, 0.000000000000000000, 1.000000000000000000 ) ) ;
#3410 = DIRECTION ( 'NONE',  ( -1.224646799147353207E-16, 1.000000000000000000, 0.000000000000000000 ) ) ;
#3411 = EDGE_LOOP ( 'NONE', ( #1854, #3110, #3055, #1293 ) ) ;
#3412 = PRESENTATION_STYLE_ASSIGNMENT (( #3066 ) ) ;
#3413 = ORIENTED_EDGE ( 'NONE', *, *, #1939, .T. ) ;
#3414 = CARTESIAN_POINT ( 'NONE',  ( 1.300000000000000044, -0.7216878364870317197, -1.250000000000000000 ) ) ;
#3415 = APPLICATION_CONTEXT ( 'automotive_design' ) ;
#3416 = EDGE_CURVE ( 'NONE', #2149, #3455, #1725, .T. ) ;
#3417 = PLANE ( 'NONE',  #2377 ) ;
#3418 = VERTEX_POINT ( 'NONE', #2328 ) ;
#3419 = CARTESIAN_POINT ( 'NONE',  ( -78.00000000000000000, 2.449293598294708880E-16, 3.000000000000000000 ) ) ;
#3420 = CARTESIAN_POINT ( 'NONE',  ( 0.000000000000000000, 0.000000000000000000, 0.000000000000000000 ) ) ;
#3421 = DIRECTION ( 'NONE',  ( 1.000000000000000000, 0.000000000000000000, 0.000000000000000000 ) ) ;
#3422 = ORIENTED_EDGE ( 'NONE', *, *, #2216, .T. ) ;
#3423 = CARTESIAN_POINT ( 'NONE',  ( 12.20000000000000107, 0.000000000000000000, 0.000000000000000000 ) ) ;
#3424 = CARTESIAN_POINT ( 'NONE',  ( -80.00000000000000000, 0.000000000000000000, 0.000000000000000000 ) ) ;
#3425 = PRESENTATION_STYLE_ASSIGNMENT (( #125 ) ) ;
#3426 = EDGE_CURVE ( 'NONE', #3229, #15, #3432, .T. ) ;
#3427 = PRODUCT_CONTEXT ( 'NONE', #2488, 'mechanical' ) ;
#3428 = DIRECTION ( 'NONE',  ( 0.000000000000000000, 0.8660254037844385966, 0.5000000000000003331 ) ) ;
#3429 = PRODUCT_DEFINITION_SHAPE ( 'NONE', 'NONE',  #1794 ) ;
#3430 = VERTEX_POINT ( 'NONE', #1665 ) ;
#3431 = CIRCLE ( 'NONE', #1752, 20.00000000000000355 ) ;
#3432 = LINE ( 'NONE', #767, #2008 ) ;
#3433 = EDGE_LOOP ( 'NONE', ( #1930, #2220 ) ) ;
#3434 = DIRECTION ( 'NONE',  ( -1.000000000000000000, 0.000000000000000000, 0.000000000000000000 ) ) ;
#3435 = UNCERTAINTY_MEASURE_WITH_UNIT (LENGTH_MEASURE( 1.000000000000000082E-05 ), #3763, 'distance_accuracy_value', 'NONE');
#3436 = CARTESIAN_POINT ( 'NONE',  ( 1.300000000000000044, 1.443375672974065216, 7.017607234860990640E-28 ) ) ;
#3437 = ORIENTED_EDGE ( 'NONE', *, *, #1897, .T. ) ;
#3438 = DIRECTION ( 'NONE',  ( 0.000000000000000000, 0.000000000000000000, 1.000000000000000000 ) ) ;
#3439 = COLOUR_RGB ( '',1.000000000000000000, 0.9490196078431372140, 0.9098039215686274384 ) ;
#3440 = DIRECTION ( 'NONE',  ( -0.000000000000000000, 0.5000000000000001110, 0.8660254037844385966 ) ) ;
#3441 = AXIS2_PLACEMENT_3D ( 'NONE', #947, #2128, #3631 ) ;
#3442 = CARTESIAN_POINT ( 'NONE',  ( 1.300000000000000044, 0.000000000000000000, 0.000000000000000000 ) ) ;
#3443 = EDGE_CURVE ( 'NONE', #2072, #328, #3562, .T. ) ;
#3444 = AXIS2_PLACEMENT_3D ( 'NONE', #2831, #713, #163 ) ;
#3445 = EDGE_LOOP ( 'NONE', ( #1857, #1084, #1001, #3682, #799, #548 ) ) ;
#3446 = FACE_BOUND ( 'NONE', #2205, .T. ) ;
#3447 = DIRECTION ( 'NONE',  ( -0.000000000000000000, -0.000000000000000000, -1.000000000000000000 ) ) ;
#3448 = CIRCLE ( 'NONE', #3196, 2.000000000000001776 ) ;
#3449 = EDGE_CURVE ( 'NONE', #1755, #910, #490, .T. ) ;
#3450 = ADVANCED_FACE ( 'NONE', ( #2290, #2107 ), #3291, .F. ) ;
#3451 = DIRECTION ( 'NONE',  ( 0.000000000000000000, 0.000000000000000000, 1.000000000000000000 ) ) ;
#3452 = VECTOR ( 'NONE', #951, 1000.000000000000000 ) ;
#3453 = MECHANICAL_DESIGN_GEOMETRIC_PRESENTATION_REPRESENTATION (  '', ( #3388 ), #2710 ) ;
#3454 = AXIS2_PLACEMENT_3D ( 'NONE', #392, #2793, #3733 ) ;
#3455 = VERTEX_POINT ( 'NONE', #2714 ) ;
#3456 = CARTESIAN_POINT ( 'NONE',  ( -83.83626752599590759, -19.67478094923029985, 1.151994720958518181 ) ) ;
#3457 = ORIENTED_EDGE ( 'NONE', *, *, #1783, .F. ) ;
#3458 = CARTESIAN_POINT ( 'NONE',  ( 8.673617379884035472E-16, 1.899999999999999689, 0.000000000000000000 ) ) ;
#3459 =( GEOMETRIC_REPRESENTATION_CONTEXT ( 3 ) GLOBAL_UNCERTAINTY_ASSIGNED_CONTEXT ( ( #828 ) ) GLOBAL_UNIT_ASSIGNED_CONTEXT ( ( #45, #3365, #3023 ) ) REPRESENTATION_CONTEXT ( 'NONE', 'WORKASPACE' ) );
#3460 = CIRCLE ( 'NONE', #913, 30.00000000000000000 ) ;
#3461 = AXIS2_PLACEMENT_3D ( 'NONE', #2742, #146, #2191 ) ;
#3462 = DIRECTION ( 'NONE',  ( 0.000000000000000000, 0.000000000000000000, -1.000000000000000000 ) ) ;
#3463 = EDGE_LOOP ( 'NONE', ( #1797, #63, #3804, #3112 ) ) ;
#3464 = CARTESIAN_POINT ( 'NONE',  ( 0.000000000000000000, 0.000000000000000000, -8.000000000000000000 ) ) ;
#3465 = CARTESIAN_POINT ( 'NONE',  ( 31.66666666666666075, 0.000000000000000000, 1.666666666666665630 ) ) ;
#3466 = ORIENTED_EDGE ( 'NONE', *, *, #3416, .T. ) ;
#3467 = DIRECTION ( 'NONE',  ( 0.000000000000000000, 0.000000000000000000, -1.000000000000000000 ) ) ;
#3468 = DIRECTION ( 'NONE',  ( -1.000000000000000000, 0.000000000000000000, 0.000000000000000000 ) ) ;
#3469 = EDGE_LOOP ( 'NONE', ( #3502, #896 ) ) ;
#3470 = CARTESIAN_POINT ( 'NONE',  ( -4.375000000000001776, -34.72548595772274638, -30.00000000000000000 ) ) ;
#3471 = ORIENTED_EDGE ( 'NONE', *, *, #2326, .T. ) ;
#3472 = ADVANCED_FACE ( 'NONE', ( #1173 ), #3003, .T. ) ;
#3473 = CARTESIAN_POINT ( 'NONE',  ( -18.99999999999999645, 0.000000000000000000, -20.00000000000000000 ) ) ;
#3474 = EDGE_LOOP ( 'NONE', ( #1439, #2797 ) ) ;
#3475 = DIRECTION ( 'NONE',  ( -1.000000000000000000, 0.000000000000000000, 0.000000000000000000 ) ) ;
#3476 = DIRECTION ( 'NONE',  ( -0.000000000000000000, 0.5000000000000001110, 0.8660254037844385966 ) ) ;
#3477 = ADVANCED_FACE ( 'NONE', ( #1796 ), #47, .T. ) ;
#3478 = ORIENTED_EDGE ( 'NONE', *, *, #1051, .T. ) ;
#3479 = CYLINDRICAL_SURFACE ( 'NONE', #2577, 18.99999999999999645 ) ;
#3480 = PRESENTATION_STYLE_ASSIGNMENT (( #1115 ) ) ;
#3481 = CARTESIAN_POINT ( 'NONE',  ( 1.300000000000000044, -0.7216878364870318308, -1.250000000000000000 ) ) ;
#3482 = DIRECTION ( 'NONE',  ( -1.000000000000000000, -0.000000000000000000, -0.000000000000000000 ) ) ;
#3483 = ORIENTED_EDGE ( 'NONE', *, *, #517, .T. ) ;
#3484 = CARTESIAN_POINT ( 'NONE',  ( -3.750000000000004441, 29.76470224947664533, 0.000000000000000000 ) ) ;
#3485 = ORIENTED_EDGE ( 'NONE', *, *, #2050, .T. ) ;
#3486 = EDGE_CURVE ( 'NONE', #1784, #2381, #3309, .T. ) ;
#3487 = AXIS2_PLACEMENT_3D ( 'NONE', #2968, #904, #607 ) ;
#3488 = DIRECTION ( 'NONE',  ( 0.000000000000000000, 0.000000000000000000, 1.000000000000000000 ) ) ;
#3489 = VERTEX_POINT ( 'NONE', #3274 ) ;
#3490 = DIRECTION ( 'NONE',  ( -0.000000000000000000, -1.000000000000000000, -0.000000000000000000 ) ) ;
#3491 = FACE_OUTER_BOUND ( 'NONE', #529, .T. ) ;
#3492 = AXIS2_PLACEMENT_3D ( 'NONE', #3602, #1512, #1231 ) ;
#3493 = AXIS2_PLACEMENT_3D ( 'NONE', #1812, #609, #2986 ) ;
#3494 = AXIS2_PLACEMENT_3D ( 'NONE', #581, #1431, #1770 ) ;
#3495 = ORIENTED_EDGE ( 'NONE', *, *, #3705, .F. ) ;
#3496 = FACE_OUTER_BOUND ( 'NONE', #306, .T. ) ;
#3497 = DIRECTION ( 'NONE',  ( -1.000000000000000000, 0.000000000000000000, 0.000000000000000000 ) ) ;
#3498 = SHAPE_REPRESENTATION_RELATIONSHIP ( 'NONE' , 'NONE' ,  #556, #2870 ) ;
#3499 = CIRCLE ( 'NONE', #1822, 7.000000000000000000 ) ;
#3500 = VECTOR ( 'NONE', #3476, 1000.000000000000000 ) ;
#3501 = UNCERTAINTY_MEASURE_WITH_UNIT (LENGTH_MEASURE( 1.000000000000000082E-05 ), #2407, 'distance_accuracy_value', 'NONE');
#3502 = ORIENTED_EDGE ( 'NONE', *, *, #2379, .T. ) ;
#3503 = AXIS2_PLACEMENT_3D ( 'NONE', #1183, #1225, #2683 ) ;
#3504 = LINE ( 'NONE', #3481, #1257 ) ;
#3505 = PRESENTATION_STYLE_ASSIGNMENT (( #1132 ) ) ;
#3506 = CARTESIAN_POINT ( 'NONE',  ( 1.300000000000000044, 0.7216878364870328300, 1.249999999999999778 ) ) ;
#3507 = ORIENTED_EDGE ( 'NONE', *, *, #2320, .T. ) ;
#3508 = EDGE_CURVE ( 'NONE', #1740, #1824, #3807, .T. ) ;
#3509 = UNCERTAINTY_MEASURE_WITH_UNIT (LENGTH_MEASURE( 1.000000000000000082E-05 ), #3759, 'distance_accuracy_value', 'NONE');
#3510 = VERTEX_POINT ( 'NONE', #2946 ) ;
#3511 = LINE ( 'NONE', #811, #2874 ) ;
#3512 = ORIENTED_EDGE ( 'NONE', *, *, #825, .T. ) ;
#3513 = CARTESIAN_POINT ( 'NONE',  ( 0.000000000000000000, 0.000000000000000000, 0.000000000000000000 ) ) ;
#3514 = EDGE_CURVE ( 'NONE', #3016, #2228, #271, .T. ) ;
#3515 =( GEOMETRIC_REPRESENTATION_CONTEXT ( 3 ) GLOBAL_UNCERTAINTY_ASSIGNED_CONTEXT ( ( #1643 ) ) GLOBAL_UNIT_ASSIGNED_CONTEXT ( ( #680, #2162, #663 ) ) REPRESENTATION_CONTEXT ( 'NONE', 'WORKASPACE' ) );
#3516 = VECTOR ( 'NONE', #2796, 1000.000000000000000 ) ;
#3517 = LINE ( 'NONE', #1447, #1879 ) ;
#3518 = CIRCLE ( 'NONE', #62, 1.324999999999999956 ) ;
#3519 = CIRCLE ( 'NONE', #598, 20.00000000000000000 ) ;
#3520 = ORIENTED_EDGE ( 'NONE', *, *, #2969, .T. ) ;
#3521 = DIRECTION ( 'NONE',  ( 0.000000000000000000, 0.000000000000000000, 1.000000000000000000 ) ) ;
#3522 =( NAMED_UNIT ( * ) SI_UNIT ( $, .STERADIAN. ) SOLID_ANGLE_UNIT ( ) );
#3523 = ORIENTED_EDGE ( 'NONE', *, *, #3045, .T. ) ;
#3524 = DIRECTION ( 'NONE',  ( -0.000000000000000000, 0.000000000000000000, 1.000000000000000000 ) ) ;
#3525 =( NAMED_UNIT ( * ) SI_UNIT ( $, .STERADIAN. ) SOLID_ANGLE_UNIT ( ) );
#3526 = CARTESIAN_POINT ( 'NONE',  ( 1.300000000000000044, 0.000000000000000000, 0.000000000000000000 ) ) ;
#3527 = EDGE_LOOP ( 'NONE', ( #3457, #1030, #1956, #1497 ) ) ;
#3528 = ORIENTED_EDGE ( 'NONE', *, *, #604, .T. ) ;
#3529 = SURFACE_STYLE_USAGE ( .BOTH. , #1161 ) ;
#3530 = ORIENTED_EDGE ( 'NONE', *, *, #2358, .F. ) ;
#3531 = LINE ( 'NONE', #1179, #403 ) ;
#3532 = EDGE_CURVE ( 'NONE', #2369, #2723, #2129, .T. ) ;
#3533 = CARTESIAN_POINT ( 'NONE',  ( 2.200000000000000178, 4.653657836759941744E-16, -3.799999999999999378 ) ) ;
#3534 =( LENGTH_UNIT ( ) NAMED_UNIT ( * ) SI_UNIT ( .MILLI., .METRE. ) );
#3535 = EDGE_LOOP ( 'NONE', ( #3138, #445, #167 ) ) ;
#3536 = DIRECTION ( 'NONE',  ( 0.000000000000000000, 0.000000000000000000, 1.000000000000000000 ) ) ;
#3537 = DIRECTION ( 'NONE',  ( 1.000000000000000000, 0.000000000000000000, 0.000000000000000000 ) ) ;
#3538 = DIRECTION ( 'NONE',  ( 0.000000000000000000, 0.000000000000000000, 1.000000000000000000 ) ) ;
#3539 = ORIENTED_EDGE ( 'NONE', *, *, #1540, .T. ) ;
#3540 = PRESENTATION_STYLE_ASSIGNMENT (( #2104 ) ) ;
#3541 = LINE ( 'NONE', #1420, #632 ) ;
#3542 = ADVANCED_FACE ( 'NONE', ( #2418 ), #3004, .T. ) ;
#3543 = CARTESIAN_POINT ( 'NONE',  ( 1.300000000000000044, 0.7216878364870328300, 1.249999999999999778 ) ) ;
#3544 = ORIENTED_EDGE ( 'NONE', *, *, #549, .T. ) ;
#3545 = AXIS2_PLACEMENT_3D ( 'NONE', #3719, #1059, #2241 ) ;
#3546 = EDGE_LOOP ( 'NONE', ( #2811, #2391, #1546 ) ) ;
#3547 = CARTESIAN_POINT ( 'NONE',  ( 1.300000000000000044, -0.7216878364870319418, 1.249999999999999778 ) ) ;
#3548 = ORIENTED_EDGE ( 'NONE', *, *, #1776, .F. ) ;
#3549 = CARTESIAN_POINT ( 'NONE',  ( 0.000000000000000000, 0.000000000000000000, -20.00000000000000355 ) ) ;
#3550 = ORIENTED_EDGE ( 'NONE', *, *, #1092, .F. ) ;
#3551 = FACE_OUTER_BOUND ( 'NONE', #31, .T. ) ;
#3552 = FACE_OUTER_BOUND ( 'NONE', #2740, .T. ) ;
#3553 = VECTOR ( 'NONE', #957, 1000.000000000000000 ) ;
#3554 = CARTESIAN_POINT ( 'NONE',  ( -82.50000000000000000, -19.84313483298442904, -30.00000000000000000 ) ) ;
#3555 = SURFACE_SIDE_STYLE ('',( #2981 ) ) ;
#3556 = EDGE_CURVE ( 'NONE', #192, #1068, #3604, .T. ) ;
#3557 = AXIS2_PLACEMENT_3D ( 'NONE', #2866, #200, #1394 ) ;
#3558 = CIRCLE ( 'NONE', #1700, 20.00000000000000000 ) ;
#3559 = VERTEX_POINT ( 'NONE', #1779 ) ;
#3560 = DIRECTION ( 'NONE',  ( -0.000000000000000000, -0.000000000000000000, -1.000000000000000000 ) ) ;
#3561 = DIRECTION ( 'NONE',  ( -0.000000000000000000, 0.4999999999999998890, -0.8660254037844387076 ) ) ;
#3562 = CIRCLE ( 'NONE', #2190, 20.00000000000000000 ) ;
#3563 = VECTOR ( 'NONE', #1673, 1000.000000000000000 ) ;
#3564 = EDGE_CURVE ( 'NONE', #2217, #1478, #1494, .T. ) ;
#3565 = EDGE_CURVE ( 'NONE', #3065, #698, #325, .T. ) ;
#3566 = AXIS2_PLACEMENT_3D ( 'NONE', #3149, #2273, #1668 ) ;
#3567 = PRODUCT ( 'MAS-190', 'MAS-190', '', ( #189 ) ) ;
#3568 = CARTESIAN_POINT ( 'NONE',  ( 0.000000000000000000, 0.000000000000000000, -30.00000000000000000 ) ) ;
#3569 = EDGE_LOOP ( 'NONE', ( #86, #2836, #1157, #3180 ) ) ;
#3570 = CIRCLE ( 'NONE', #451, 0.2000000000000000944 ) ;
#3571 = ORIENTED_EDGE ( 'NONE', *, *, #835, .T. ) ;
#3572 = DIRECTION ( 'NONE',  ( -1.000000000000000000, 1.776356839400250070E-15, 0.000000000000000000 ) ) ;
#3573 = ORIENTED_EDGE ( 'NONE', *, *, #516, .F. ) ;
#3574 = LINE ( 'NONE', #2681, #1828 ) ;
#3575 = VECTOR ( 'NONE', #1876, 1000.000000000000000 ) ;
#3576 = PRODUCT_DEFINITION ( 'UNKNOWN', '', #2531, #2890 ) ;
#3577 = COLOUR_RGB ( '',1.000000000000000000, 0.9490196078431372140, 0.9098039215686274384 ) ;
#3578 = CONTEXT_DEPENDENT_SHAPE_REPRESENTATION ( #2615, #3297 ) ;
#3579 = ORIENTED_EDGE ( 'NONE', *, *, #2064, .T. ) ;
#3580 = DIRECTION ( 'NONE',  ( -0.000000000000000000, 1.000000000000000000, -0.000000000000000000 ) ) ;
#3581 = DIRECTION ( 'NONE',  ( 0.000000000000000000, 0.000000000000000000, 1.000000000000000000 ) ) ;
#3582 = FILL_AREA_STYLE ('',( #1039 ) ) ;
#3583 = VECTOR ( 'NONE', #2953, 1000.000000000000000 ) ;
#3584 = EDGE_LOOP ( 'NONE', ( #3233, #3579, #1890, #2651 ) ) ;
#3585 = SURFACE_SIDE_STYLE ('',( #2361 ) ) ;
#3586 = CIRCLE ( 'NONE', #2083, 25.15000000000000213 ) ;
#3587 = CARTESIAN_POINT ( 'NONE',  ( 4.336808689942017736E-16, 0.000000000000000000, 0.000000000000000000 ) ) ;
#3588 = FILL_AREA_STYLE ('',( #2690 ) ) ;
#3589 = DIRECTION ( 'NONE',  ( -1.000000000000000000, -0.000000000000000000, -0.000000000000000000 ) ) ;
#3590 = ORIENTED_EDGE ( 'NONE', *, *, #2353, .F. ) ;
#3591 = VERTEX_POINT ( 'NONE', #27 ) ;
#3592 = ORIENTED_EDGE ( 'NONE', *, *, #2311, .T. ) ;
#3593 = DIRECTION ( 'NONE',  ( -1.000000000000000000, 0.000000000000000000, 0.000000000000000000 ) ) ;
#3594 = EDGE_CURVE ( 'NONE', #3489, #2587, #2927, .T. ) ;
#3595 = ORIENTED_EDGE ( 'NONE', *, *, #3045, .F. ) ;
#3596 = DIRECTION ( 'NONE',  ( 0.000000000000000000, -0.000000000000000000, -1.000000000000000000 ) ) ;
#3597 = DIRECTION ( 'NONE',  ( -0.000000000000000000, 0.000000000000000000, 1.000000000000000000 ) ) ;
#3598 = FILL_AREA_STYLE_COLOUR ( '', #130 ) ;
#3599 = CARTESIAN_POINT ( 'NONE',  ( -80.00000000000000000, 2.220707773205301361E-16, -8.800000000000000711 ) ) ;
#3600 = EDGE_CURVE ( 'NONE', #1136, #1813, #2131, .T. ) ;
#3601 = DIRECTION ( 'NONE',  ( -1.000000000000000000, 0.000000000000000000, 0.000000000000000000 ) ) ;
#3602 = CARTESIAN_POINT ( 'NONE',  ( -80.00000000000000000, 0.000000000000000000, 3.000000000000000000 ) ) ;
#3603 = FACE_OUTER_BOUND ( 'NONE', #2278, .T. ) ;
#3604 = LINE ( 'NONE', #3217, #3132 ) ;
#3605 = EDGE_LOOP ( 'NONE', ( #3295, #1629, #2929, #1366, #1816 ) ) ;
#3606 = EDGE_CURVE ( 'NONE', #3147, #3210, #3190, .T. ) ;
#3607 = ORIENTED_EDGE ( 'NONE', *, *, #825, .F. ) ;
#3608 = FILL_AREA_STYLE_COLOUR ( '', #1699 ) ;
#3610 = ORIENTED_EDGE ( 'NONE', *, *, #1849, .F. ) ;
#3609 = EDGE_CURVE ( 'NONE', #691, #1187, #139, .T. ) ;
#3611 = DIRECTION ( 'NONE',  ( 0.000000000000000000, 0.000000000000000000, 1.000000000000000000 ) ) ;
#3612 = PRODUCT ( 'plain washer 10669 type nl_iso_ISO 10669-5.4-N', 'plain washer 10669 type nl_iso_ISO 10669-5.4-N', '', ( #1659 ) ) ;
#3613 = EDGE_CURVE ( 'NONE', #137, #1, #872, .T. ) ;
#3614 = EDGE_CURVE ( 'NONE', #1238, #1374, #449, .T. ) ;
#3615 = VERTEX_POINT ( 'NONE', #2769 ) ;
#3616 = FACE_OUTER_BOUND ( 'NONE', #1464, .T. ) ;
#3617 = FACE_OUTER_BOUND ( 'NONE', #1645, .T. ) ;
#3618 = CARTESIAN_POINT ( 'NONE',  ( 1.300000000000000044, 0.7216878364870328300, -1.250000000000000000 ) ) ;
#3619 = UNCERTAINTY_MEASURE_WITH_UNIT (LENGTH_MEASURE( 1.000000000000000082E-05 ), #884, 'distance_accuracy_value', 'NONE');
#3620 = AXIS2_PLACEMENT_3D ( 'NONE', #2362, #565, #2305 ) ;
#3621 = CARTESIAN_POINT ( 'NONE',  ( 20.74496707014011676, -8.711850621928872940, 0.000000000000000000 ) ) ;
#3622 = LINE ( 'NONE', #979, #3553 ) ;
#3623 = AXIS2_PLACEMENT_3D ( 'NONE', #1845, #1507, #1549 ) ;
#3624 = AXIS2_PLACEMENT_3D ( 'NONE', #3568, #2970, #1233 ) ;
#3625 = AXIS2_PLACEMENT_3D ( 'NONE', #931, #354, #3611 ) ;
#3626 = CARTESIAN_POINT ( 'NONE',  ( 1.300000000000000044, -1.443375672974063884, -3.691112476943992763E-18 ) ) ;
#3627 = DIRECTION ( 'NONE',  ( 1.000000000000000000, 0.000000000000000000, 0.000000000000000000 ) ) ;
#3628 = EDGE_LOOP ( 'NONE', ( #1941, #601 ) ) ;
#3629 = VERTEX_POINT ( 'NONE', #3368 ) ;
#3630 = AXIS2_PLACEMENT_3D ( 'NONE', #3343, #3072, #369 ) ;
#3631 = DIRECTION ( 'NONE',  ( -1.000000000000000000, 0.000000000000000000, 0.000000000000000000 ) ) ;
#3632 = ORIENTED_EDGE ( 'NONE', *, *, #1777, .T. ) ;
#3633 = DIRECTION ( 'NONE',  ( 0.000000000000000000, 0.000000000000000000, 1.000000000000000000 ) ) ;
#3634 = CARTESIAN_POINT ( 'NONE',  ( 0.000000000000000000, 1.443375672974065216, 7.017607234860990640E-28 ) ) ;
#3635 = FACE_OUTER_BOUND ( 'NONE', #2975, .T. ) ;
#3636 = AXIS2_PLACEMENT_3D ( 'NONE', #729, #1835, #61 ) ;
#3637 = AXIS2_PLACEMENT_3D ( 'NONE', #1313, #119, #3131 ) ;
#3638 = CYLINDRICAL_SURFACE ( 'NONE', #2827, 1.999999999999999112 ) ;
#3639 = DIRECTION ( 'NONE',  ( 0.000000000000000000, -0.000000000000000000, -1.000000000000000000 ) ) ;
#3640 = CIRCLE ( 'NONE', #3828, 1.899999999999999689 ) ;
#3641 = CARTESIAN_POINT ( 'NONE',  ( -80.00000000000000000, 0.000000000000000000, -5.000000000000000000 ) ) ;
#3642 = FACE_OUTER_BOUND ( 'NONE', #3393, .T. ) ;
#3643 = PRODUCT ( 'shuttle unit', 'shuttle unit', '', ( #1948 ) ) ;
#3644 = EDGE_CURVE ( 'NONE', #385, #2723, #2817, .T. ) ;
#3645 = VERTEX_POINT ( 'NONE', #706 ) ;
#3646 = SURFACE_STYLE_USAGE ( .BOTH. , #2457 ) ;
#3647 = ORIENTED_EDGE ( 'NONE', *, *, #1121, .T. ) ;
#3648 = CARTESIAN_POINT ( 'NONE',  ( 4.336808689942017736E-16, -0.7216878364870317197, 1.250000000000000000 ) ) ;
#3649 = EDGE_CURVE ( 'NONE', #2084, #1107, #3086, .T. ) ;
#3650 = DIRECTION ( 'NONE',  ( 0.1250000000000001665, -0.9921567416492215186, 0.000000000000000000 ) ) ;
#3651 = EDGE_LOOP ( 'NONE', ( #2734, #753, #2383, #613 ) ) ;
#3652 = DIRECTION ( 'NONE',  ( 0.000000000000000000, 0.000000000000000000, -1.000000000000000000 ) ) ;
#3653 = CARTESIAN_POINT ( 'NONE',  ( 21.96661513093725659, -9.224881825220240472, -2.544523588129261943E-16 ) ) ;
#3654 = DIRECTION ( 'NONE',  ( 0.3736424900038657904, -0.8444627602987255788, 0.3837628644519533450 ) ) ;
#3655 = CARTESIAN_POINT ( 'NONE',  ( 2.200000000000000178, 0.000000000000000000, 0.000000000000000000 ) ) ;
#3656 = FACE_OUTER_BOUND ( 'NONE', #655, .T. ) ;
#3657 = FILL_AREA_STYLE_COLOUR ( '', #2145 ) ;
#3658 = EDGE_CURVE ( 'NONE', #208, #1281, #2327, .T. ) ;
#3659 = DIRECTION ( 'NONE',  ( 0.000000000000000000, 0.4999999999999999445, 0.8660254037844387076 ) ) ;
#3660 = DIRECTION ( 'NONE',  ( -0.000000000000000000, -0.000000000000000000, -1.000000000000000000 ) ) ;
#3661 = ORIENTED_EDGE ( 'NONE', *, *, #100, .T. ) ;
#3662 = SURFACE_STYLE_FILL_AREA ( #1615 ) ;
#3663 = ORIENTED_EDGE ( 'NONE', *, *, #2989, .F. ) ;
#3664 = FACE_OUTER_BOUND ( 'NONE', #3225, .T. ) ;
#3665 = LINE ( 'NONE', #1280, #708 ) ;
#3666 = VERTEX_POINT ( 'NONE', #3047 ) ;
#3667 = CARTESIAN_POINT ( 'NONE',  ( -75.00000000000000000, 6.123233995736772199E-16, 0.000000000000000000 ) ) ;
#3668 = DIRECTION ( 'NONE',  ( 0.9219985364506716463, -0.3871933609746164295, 0.000000000000000000 ) ) ;
#3669 = DIRECTION ( 'NONE',  ( 0.000000000000000000, 0.000000000000000000, -1.000000000000000000 ) ) ;
#3670 = FACE_OUTER_BOUND ( 'NONE', #506, .T. ) ;
#3671 = ORIENTED_EDGE ( 'NONE', *, *, #1000, .F. ) ;
#3672 = ADVANCED_FACE ( 'NONE', ( #3642 ), #112, .T. ) ;
#3673 = LINE ( 'NONE', #1882, #2258 ) ;
#3674 = APPLICATION_PROTOCOL_DEFINITION ( 'draft international standard', 'automotive_design', 1998, #3170 ) ;
#3675 = CARTESIAN_POINT ( 'NONE',  ( 0.000000000000000000, 0.000000000000000000, 0.000000000000000000 ) ) ;
#3676 = CARTESIAN_POINT ( 'NONE',  ( 1.820000000000000062, 0.000000000000000000, 0.000000000000000000 ) ) ;
#3677 = AXIS2_PLACEMENT_3D ( 'NONE', #1456, #1492, #1211 ) ;
#3678 = EDGE_CURVE ( 'NONE', #52, #1782, #1323, .T. ) ;
#3679 = EDGE_CURVE ( 'NONE', #3156, #535, #983, .T. ) ;
#3680 = AXIS2_PLACEMENT_3D ( 'NONE', #3470, #2271, #806 ) ;
#3681 = COLOUR_RGB ( '',0.8941176470588234615, 0.8941176470588234615, 0.8941176470588234615 ) ;
#3682 = ORIENTED_EDGE ( 'NONE', *, *, #3565, .T. ) ;
#3683 = ORIENTED_EDGE ( 'NONE', *, *, #1525, .T. ) ;
#3684 = FACE_BOUND ( 'NONE', #1687, .T. ) ;
#3685 = AXIS2_PLACEMENT_3D ( 'NONE', #3526, #3589, #925 ) ;
#3686 = CIRCLE ( 'NONE', #3251, 1.249999999999999778 ) ;
#3687 = VECTOR ( 'NONE', #2156, 1000.000000000000000 ) ;
#3688 = CYLINDRICAL_SURFACE ( 'NONE', #3078, 7.000000000000000000 ) ;
#3689 = ORIENTED_EDGE ( 'NONE', *, *, #151, .T. ) ;
#3690 = DIRECTION ( 'NONE',  ( 0.000000000000000000, 0.000000000000000000, 1.000000000000000000 ) ) ;
#3691 = PLANE ( 'NONE',  #1590 ) ;
#3692 = CARTESIAN_POINT ( 'NONE',  ( 2.000000000000001776, 2.449293598294708880E-16, -30.00000000000000000 ) ) ;
#3693 = EDGE_CURVE ( 'NONE', #2736, #201, #3499, .T. ) ;
#3694 = CONICAL_SURFACE ( 'NONE', #771, 1.649999999999998579, 1.029744258676653423 ) ;
#3695 = DIRECTION ( 'NONE',  ( 1.000000000000000000, 0.000000000000000000, 0.000000000000000000 ) ) ;
#3696 = DIRECTION ( 'NONE',  ( 1.000000000000000000, 0.000000000000000000, 0.000000000000000000 ) ) ;
#3697 = CARTESIAN_POINT ( 'NONE',  ( -997.9783121635130101, 0.000000000000000000, 0.000000000000000000 ) ) ;
#3698 = VECTOR ( 'NONE', #3000, 1000.000000000000000 ) ;
#3699 = CONTEXT_DEPENDENT_SHAPE_REPRESENTATION ( #3362, #1072 ) ;
#3700 = EDGE_CURVE ( 'NONE', #2659, #2253, #421, .T. ) ;
#3701 = AXIS2_PLACEMENT_3D ( 'NONE', #1554, #1661, #471 ) ;
#3702 = VECTOR ( 'NONE', #2189, 1000.000000000000000 ) ;
#3703 = DIRECTION ( 'NONE',  ( 0.000000000000000000, 0.000000000000000000, 1.000000000000000000 ) ) ;
#3704 = CYLINDRICAL_SURFACE ( 'NONE', #528, 20.00000000000000000 ) ;
#3705 = EDGE_CURVE ( 'NONE', #1408, #1346, #683, .T. ) ;
#3706 = CIRCLE ( 'NONE', #1584, 20.00000000000000355 ) ;
#3707 = ORIENTED_EDGE ( 'NONE', *, *, #2283, .T. ) ;
#3708 = DIRECTION ( 'NONE',  ( 0.000000000000000000, 0.000000000000000000, -1.000000000000000000 ) ) ;
#3709 = ORIENTED_EDGE ( 'NONE', *, *, #3678, .T. ) ;
#3710 = CARTESIAN_POINT ( 'NONE',  ( 2.399999999999999911, 0.000000000000000000, 0.000000000000000000 ) ) ;
#3711 = UNCERTAINTY_MEASURE_WITH_UNIT (LENGTH_MEASURE( 1.000000000000000082E-05 ), #823, 'distance_accuracy_value', 'NONE');
#3712 = DIRECTION ( 'NONE',  ( 0.000000000000000000, 0.000000000000000000, -1.000000000000000000 ) ) ;
#3713 = ORIENTED_EDGE ( 'NONE', *, *, #422, .F. ) ;
#3714 = SPHERICAL_SURFACE ( 'NONE', #2582, 4.324969328314201888 ) ;
#3715 = DIRECTION ( 'NONE',  ( -1.000000000000000000, -0.000000000000000000, -0.000000000000000000 ) ) ;
#3716 = DIRECTION ( 'NONE',  ( 0.000000000000000000, 0.000000000000000000, 1.000000000000000000 ) ) ;
#3717 = ADVANCED_FACE ( 'NONE', ( #2454 ), #3704, .F. ) ;
#3718 = DIRECTION ( 'NONE',  ( 0.000000000000000000, 0.000000000000000000, 1.000000000000000000 ) ) ;
#3719 = CARTESIAN_POINT ( 'NONE',  ( 0.000000000000000000, 0.000000000000000000, 1.102182119232617788E-16 ) ) ;
#3720 = DIRECTION ( 'NONE',  ( 1.000000000000000000, 0.000000000000000000, 0.000000000000000000 ) ) ;
#3721 = SHAPE_REPRESENTATION_RELATIONSHIP ( 'NONE' , 'NONE' ,  #3744, #1526 ) ;
#3722 = ADVANCED_FACE ( 'NONE', ( #1595 ), #3063, .F. ) ;
#3723 = DIRECTION ( 'NONE',  ( 0.000000000000000000, 1.000000000000000000, 1.224646799147353454E-16 ) ) ;
#3724 = ORIENTED_EDGE ( 'NONE', *, *, #304, .F. ) ;
#3725 = DIRECTION ( 'NONE',  ( -0.000000000000000000, -0.000000000000000000, -1.000000000000000000 ) ) ;
#3726 = ORIENTED_EDGE ( 'NONE', *, *, #1827, .F. ) ;
#3727 = FACE_OUTER_BOUND ( 'NONE', #3584, .T. ) ;
#3728 = EDGE_CURVE ( 'NONE', #1003, #2595, #3391, .T. ) ;
#3729 = EDGE_CURVE ( 'NONE', #1740, #3235, #1517, .T. ) ;
#3730 = EDGE_CURVE ( 'NONE', #1813, #2170, #2028, .T. ) ;
#3731 = PLANE ( 'NONE',  #903 ) ;
#3732 = ORIENTED_EDGE ( 'NONE', *, *, #1051, .F. ) ;
#3733 = DIRECTION ( 'NONE',  ( 0.000000000000000000, 0.000000000000000000, 1.000000000000000000 ) ) ;
#3734 = DIRECTION ( 'NONE',  ( 0.000000000000000000, 0.000000000000000000, 1.000000000000000000 ) ) ;
#3735 = DIRECTION ( 'NONE',  ( -0.000000000000000000, -0.000000000000000000, -1.000000000000000000 ) ) ;
#3736 = EDGE_CURVE ( 'NONE', #1528, #3430, #3030, .T. ) ;
#3737 = EDGE_CURVE ( 'NONE', #2422, #2309, #1962, .T. ) ;
#3738 = ORIENTED_EDGE ( 'NONE', *, *, #854, .T. ) ;
#3739 = DIRECTION ( 'NONE',  ( 0.000000000000000000, 0.000000000000000000, 1.000000000000000000 ) ) ;
#3740 = DIRECTION ( 'NONE',  ( 0.000000000000000000, 0.000000000000000000, 1.000000000000000000 ) ) ;
#3741 =( LENGTH_UNIT ( ) NAMED_UNIT ( * ) SI_UNIT ( .MILLI., .METRE. ) );
#3742 = SHAPE_DEFINITION_REPRESENTATION ( #2803, #3744 ) ;
#3743 = DIRECTION ( 'NONE',  ( -1.795453617517838654E-17, 1.015442787603507153E-17, 1.000000000000000000 ) ) ;
#3744 = SHAPE_REPRESENTATION ( 'socket button head screw_iso_ISO 7380 - M4 x 8 - 8N', ( #2207 ), #2713 ) ;
#3745 = ORIENTED_EDGE ( 'NONE', *, *, #1820, .F. ) ;
#3746 = CIRCLE ( 'NONE', #2186, 5.000000000000004441 ) ;
#3747 = CARTESIAN_POINT ( 'NONE',  ( 0.000000000000000000, 0.000000000000000000, -20.00000000000000000 ) ) ;
#3748 = ORIENTED_EDGE ( 'NONE', *, *, #564, .T. ) ;
#3749 = DIRECTION ( 'NONE',  ( -1.000000000000000000, 0.000000000000000000, 0.000000000000000000 ) ) ;
#3750 = AXIS2_PLACEMENT_3D ( 'NONE', #2357, #3810, #2622 ) ;
#3751 = CARTESIAN_POINT ( 'NONE',  ( 0.000000000000000000, 0.000000000000000000, 0.000000000000000000 ) ) ;
#3752 = VERTEX_POINT ( 'NONE', #2180 ) ;
#3753 = DIRECTION ( 'NONE',  ( 1.000000000000000000, 0.000000000000000000, 0.000000000000000000 ) ) ;
#3754 = COLOUR_RGB ( '',0.8941176470588234615, 0.8941176470588234615, 0.8941176470588234615 ) ;
#3755 = LINE ( 'NONE', #3827, #3500 ) ;
#3756 = AXIS2_PLACEMENT_3D ( 'NONE', #2392, #3284, #2100 ) ;
#3757 = ORIENTED_EDGE ( 'NONE', *, *, #2019, .T. ) ;
#3758 = LINE ( 'NONE', #1038, #822 ) ;
#3759 =( LENGTH_UNIT ( ) NAMED_UNIT ( * ) SI_UNIT ( .MILLI., .METRE. ) );
#3760 = CIRCLE ( 'NONE', #2635, 1.610000000000000098 ) ;
#3761 = APPLICATION_PROTOCOL_DEFINITION ( 'draft international standard', 'automotive_design', 1998, #2488 ) ;
#3762 = CARTESIAN_POINT ( 'NONE',  ( 1.300000000000000044, -1.443375672974063884, -3.691112476943992763E-18 ) ) ;
#3763 =( LENGTH_UNIT ( ) NAMED_UNIT ( * ) SI_UNIT ( .MILLI., .METRE. ) );
#3764 = AXIS2_PLACEMENT_3D ( 'NONE', #3265, #2647, #3285 ) ;
#3765 = EDGE_CURVE ( 'NONE', #1782, #52, #2766, .T. ) ;
#3766 = APPLICATION_CONTEXT ( 'automotive_design' ) ;
#3767 = VECTOR ( 'NONE', #2429, 1000.000000000000114 ) ;
#3768 = ORIENTED_EDGE ( 'NONE', *, *, #562, .T. ) ;
#3769 = PLANE ( 'NONE',  #1756 ) ;
#3770 = ORIENTED_EDGE ( 'NONE', *, *, #3564, .T. ) ;
#3771 = AXIS2_PLACEMENT_3D ( 'NONE', #1553, #3085, #2768 ) ;
#3772 = EDGE_CURVE ( 'NONE', #1374, #1238, #1097, .T. ) ;
#3773 = AXIS2_PLACEMENT_3D ( 'NONE', #89, #1033, #1056 ) ;
#3774 = PLANE ( 'NONE',  #327 ) ;
#3775 = ORIENTED_EDGE ( 'NONE', *, *, #564, .F. ) ;
#3776 = DIRECTION ( 'NONE',  ( 1.000000000000000000, 0.000000000000000000, -0.000000000000000000 ) ) ;
#3777 = PLANE ( 'NONE',  #1199 ) ;
#3778 = EDGE_CURVE ( 'NONE', #2365, #2698, #333, .T. ) ;
#3779 = ORIENTED_EDGE ( 'NONE', *, *, #1009, .F. ) ;
#3780 = LINE ( 'NONE', #1675, #1781 ) ;
#3781 = SURFACE_SIDE_STYLE ('',( #2877 ) ) ;
#3782 = EDGE_CURVE ( 'NONE', #926, #1166, #269, .T. ) ;
#3783 = DIRECTION ( 'NONE',  ( -1.000000000000000000, 0.000000000000000000, 0.000000000000000000 ) ) ;
#3784 = CARTESIAN_POINT ( 'NONE',  ( 30.95238095238181231, 5.297284633636610174, 5.000000000000000000 ) ) ;
#3785 = VERTEX_POINT ( 'NONE', #2294 ) ;
#3786 = CARTESIAN_POINT ( 'NONE',  ( -88.76305748969319609, -18.02152214568556943, 4.485328054291851885 ) ) ;
#3787 = ORIENTED_EDGE ( 'NONE', *, *, #2019, .F. ) ;
#3788 = CARTESIAN_POINT ( 'NONE',  ( 0.000000000000000000, -0.7216878364870318308, -1.250000000000000000 ) ) ;
#3789 = ORIENTED_EDGE ( 'NONE', *, *, #867, .T. ) ;
#3790 = CARTESIAN_POINT ( 'NONE',  ( 1.300000000000000044, -0.7216878364870318308, 1.249999999999999778 ) ) ;
#3791 = LINE ( 'NONE', #2334, #2695 ) ;
#3792 = EDGE_LOOP ( 'NONE', ( #3808, #312 ) ) ;
#3793 = LINE ( 'NONE', #1730, #2405 ) ;
#3794 = CARTESIAN_POINT ( 'NONE',  ( 0.000000000000000000, 0.000000000000000000, 0.000000000000000000 ) ) ;
#3795 =( LENGTH_UNIT ( ) NAMED_UNIT ( * ) SI_UNIT ( .MILLI., .METRE. ) );
#3796 = EDGE_CURVE ( 'NONE', #328, #2072, #2516, .T. ) ;
#3797 = ORIENTED_EDGE ( 'NONE', *, *, #1410, .F. ) ;
#3798 = CARTESIAN_POINT ( 'NONE',  ( 2.021687836487040535, 2.168404344971008868E-16, 0.000000000000000000 ) ) ;
#3799 = SURFACE_STYLE_FILL_AREA ( #545 ) ;
#3800 = ORIENTED_EDGE ( 'NONE', *, *, #106, .T. ) ;
#3801 = EDGE_CURVE ( 'NONE', #3235, #1740, #846, .T. ) ;
#3802 = AXIS2_PLACEMENT_3D ( 'NONE', #2534, #485, #2552 ) ;
#3803 = CARTESIAN_POINT ( 'NONE',  ( 2.400000000000000799, 2.694222958124176020E-16, -2.199999999999999289 ) ) ;
#3804 = ORIENTED_EDGE ( 'NONE', *, *, #2353, .T. ) ;
#3805 = CARTESIAN_POINT ( 'NONE',  ( 2.399999999999999911, 0.000000000000000000, 2.199999999999999289 ) ) ;
#3806 = PLANE ( 'NONE',  #895 ) ;
#3807 = CIRCLE ( 'NONE', #258, 25.15000000000000213 ) ;
#3808 = ORIENTED_EDGE ( 'NONE', *, *, #2922, .T. ) ;
#3809 = CARTESIAN_POINT ( 'NONE',  ( -2.000000000000001776, 0.000000000000000000, -20.00000000000000000 ) ) ;
#3810 = DIRECTION ( 'NONE',  ( -1.224646799147353207E-16, 1.000000000000000000, 0.000000000000000000 ) ) ;
#3811 =( NAMED_UNIT ( * ) SI_UNIT ( $, .STERADIAN. ) SOLID_ANGLE_UNIT ( ) );
#3812 = AXIS2_PLACEMENT_3D ( 'NONE', #2432, #1865, #1250 ) ;
#3813 = AXIS2_PLACEMENT_3D ( 'NONE', #1817, #2151, #2976 ) ;
#3814 = ORIENTED_EDGE ( 'NONE', *, *, #1785, .T. ) ;
#3815 = DIRECTION ( 'NONE',  ( -0.000000000000000000, -0.000000000000000000, -1.000000000000000000 ) ) ;
#3816 =( LENGTH_UNIT ( ) NAMED_UNIT ( * ) SI_UNIT ( .MILLI., .METRE. ) );
#3817 = PRODUCT_RELATED_PRODUCT_CATEGORY ( 'part', '', ( #343 ) ) ;
#3818 = CARTESIAN_POINT ( 'NONE',  ( 1.820000000000000062, 0.000000000000000000, 0.000000000000000000 ) ) ;
#3819 = ORIENTED_EDGE ( 'NONE', *, *, #1785, .F. ) ;
#3820 = STYLED_ITEM ( 'NONE', ( #3505 ), #2924 ) ;
#3821 = VECTOR ( 'NONE', #3060, 1000.000000000000000 ) ;
#3822 = VERTEX_POINT ( 'NONE', #156 ) ;
#3823 = CARTESIAN_POINT ( 'NONE',  ( 1.300000000000000044, -0.7216878364870317197, 1.250000000000000000 ) ) ;
#3824 = VERTEX_POINT ( 'NONE', #2905 ) ;
#3825 = FACE_OUTER_BOUND ( 'NONE', #1442, .T. ) ;
#3826 = CIRCLE ( 'NONE', #2341, 4.324969328314201888 ) ;
#3827 = CARTESIAN_POINT ( 'NONE',  ( 0.000000000000000000, 1.443375672974065216, 7.017607234860990640E-28 ) ) ;
#3828 = AXIS2_PLACEMENT_3D ( 'NONE', #1968, #2260, #2317 ) ;
#3829 = ADVANCED_FACE ( 'NONE', ( #1117 ), #1350, .T. ) ;
#3830 = APPLICATION_PROTOCOL_DEFINITION ( 'draft international standard', 'automotive_design', 1998, #1175 ) ;
#3831 = EDGE_LOOP ( 'NONE', ( #2040, #1993 ) ) ;
#3832 = DIRECTION ( 'NONE',  ( -0.000000000000000000, -0.000000000000000000, -1.000000000000000000 ) ) ;
#3833 = CARTESIAN_POINT ( 'NONE',  ( -89.85223847358115279, -17.40498196091244409, 5.000000000000000000 ) ) ;
#3834 =( NAMED_UNIT ( * ) PLANE_ANGLE_UNIT ( ) SI_UNIT ( $, .RADIAN. ) );
#3835 = ORIENTED_EDGE ( 'NONE', *, *, #2388, .F. ) ;
#3836 = FILL_AREA_STYLE_COLOUR ( '', #3577 ) ;
#3837 = DIRECTION ( 'NONE',  ( 0.000000000000000000, 0.000000000000000000, -1.000000000000000000 ) ) ;
#3838 = LINE ( 'NONE', #53, #75 ) ;
#3839 = NEXT_ASSEMBLY_USAGE_OCCURRENCE ( 'NAUO1', ' ', ' ', #899, #1794, $ ) ;
#3840 = NEXT_ASSEMBLY_USAGE_OCCURRENCE ( 'NAUO2', ' ', ' ', #899, #583, $ ) ;
#3841 = NEXT_ASSEMBLY_USAGE_OCCURRENCE ( 'NAUO3', ' ', ' ', #899, #3576, $ ) ;
#3842 = NEXT_ASSEMBLY_USAGE_OCCURRENCE ( 'NAUO4', ' ', ' ', #899, #537, $ ) ;
#3843 = NEXT_ASSEMBLY_USAGE_OCCURRENCE ( 'NAUO5', ' ', ' ', #899, #1232, $ ) ;
#3844 = NEXT_ASSEMBLY_USAGE_OCCURRENCE ( 'NAUO6', ' ', ' ', #899, #1705, $ ) ;
#3845 = NEXT_ASSEMBLY_USAGE_OCCURRENCE ( 'NAUO7', ' ', ' ', #899, #2395, $ ) ;
#3846 = NEXT_ASSEMBLY_USAGE_OCCURRENCE ( 'NAUO8', ' ', ' ', #899, #3366, $ ) ;
#3847=COLOUR_RGB('Dark Blue',0.08,0.2,0.34);
#3848=FILL_AREA_STYLE_COLOUR('',#3847);
#3849=FILL_AREA_STYLE('',(#3848));
#3850=SURFACE_STYLE_FILL_AREA(#3849);
#3851=SURFACE_SIDE_STYLE('',(#3850));
#3852=SURFACE_STYLE_USAGE(.BOTH.,#3851);
#3853=PRESENTATION_STYLE_ASSIGNMENT((#3852));
#3854=COLOUR_RGB('Light Blue',0.38,0.62,0.78);
#3855=FILL_AREA_STYLE_COLOUR('',#3854);
#3856=FILL_AREA_STYLE('',(#3855));
#3857=SURFACE_STYLE_FILL_AREA(#3856);
#3858=SURFACE_SIDE_STYLE('',(#3857));
#3859=SURFACE_STYLE_USAGE(.BOTH.,#3858);
#3860=PRESENTATION_STYLE_ASSIGNMENT((#3859));
#3861=COLOUR_RGB('Sky Blue',0.24,0.69,0.87);
#3862=FILL_AREA_STYLE_COLOUR('',#3861);
#3863=FILL_AREA_STYLE('',(#3862));
#3864=SURFACE_STYLE_FILL_AREA(#3863);
#3865=SURFACE_SIDE_STYLE('',(#3864));
#3866=SURFACE_STYLE_USAGE(.BOTH.,#3865);
#3867=PRESENTATION_STYLE_ASSIGNMENT((#3866));
#3868=COLOUR_RGB('Grey',0.48,0.52,0.57);
#3869=FILL_AREA_STYLE_COLOUR('',#3868);
#3870=FILL_AREA_STYLE('',(#3869));
#3871=SURFACE_STYLE_FILL_AREA(#3870);
#3872=SURFACE_SIDE_STYLE('',(#3871));
#3873=SURFACE_STYLE_USAGE(.BOTH.,#3872);
#3874=PRESENTATION_STYLE_ASSIGNMENT((#3873));
#3875=COLOUR_RGB('Black',0.12,0.14,0.17);
#3876=FILL_AREA_STYLE_COLOUR('',#3875);
#3877=FILL_AREA_STYLE('',(#3876));
#3878=SURFACE_STYLE_FILL_AREA(#3877);
#3879=SURFACE_SIDE_STYLE('',(#3878));
#3880=SURFACE_STYLE_USAGE(.BOTH.,#3879);
#3881=PRESENTATION_STYLE_ASSIGNMENT((#3880));
#3882=COLOUR_RGB('Off White',0.89,0.88,0.83);
#3883=FILL_AREA_STYLE_COLOUR('',#3882);
#3884=FILL_AREA_STYLE('',(#3883));
#3885=SURFACE_STYLE_FILL_AREA(#3884);
#3886=SURFACE_SIDE_STYLE('',(#3885));
#3887=SURFACE_STYLE_USAGE(.BOTH.,#3886);
#3888=PRESENTATION_STYLE_ASSIGNMENT((#3887));
ENDSEC;
END-ISO-10303-21;
